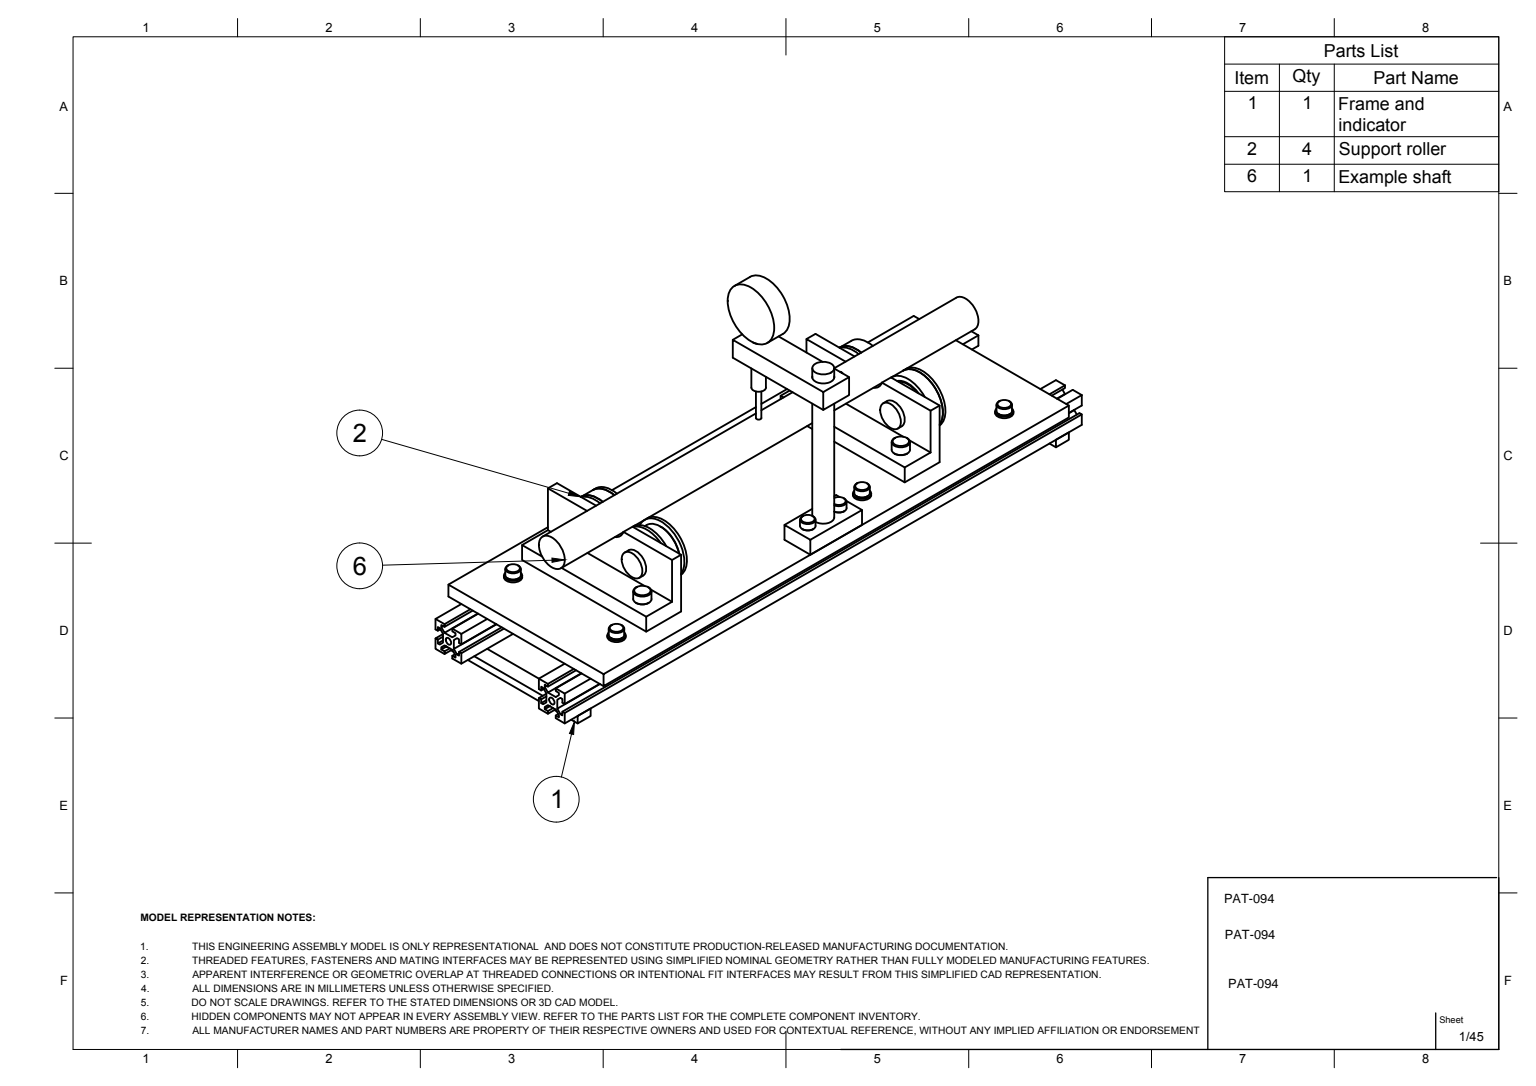
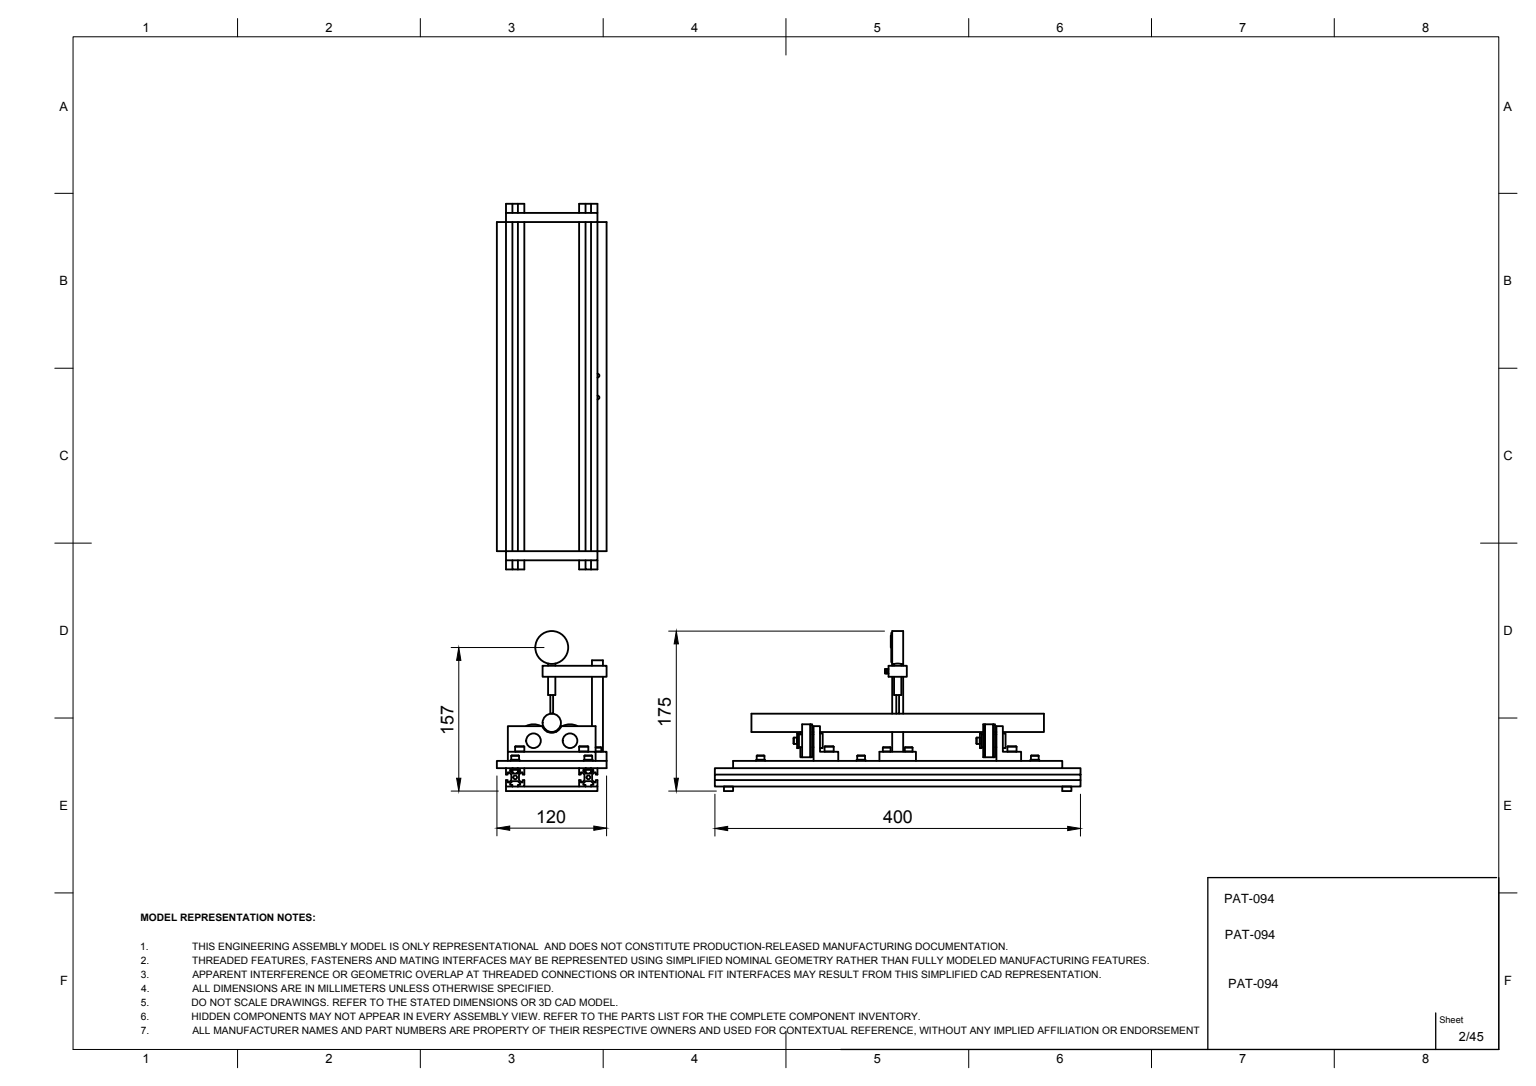
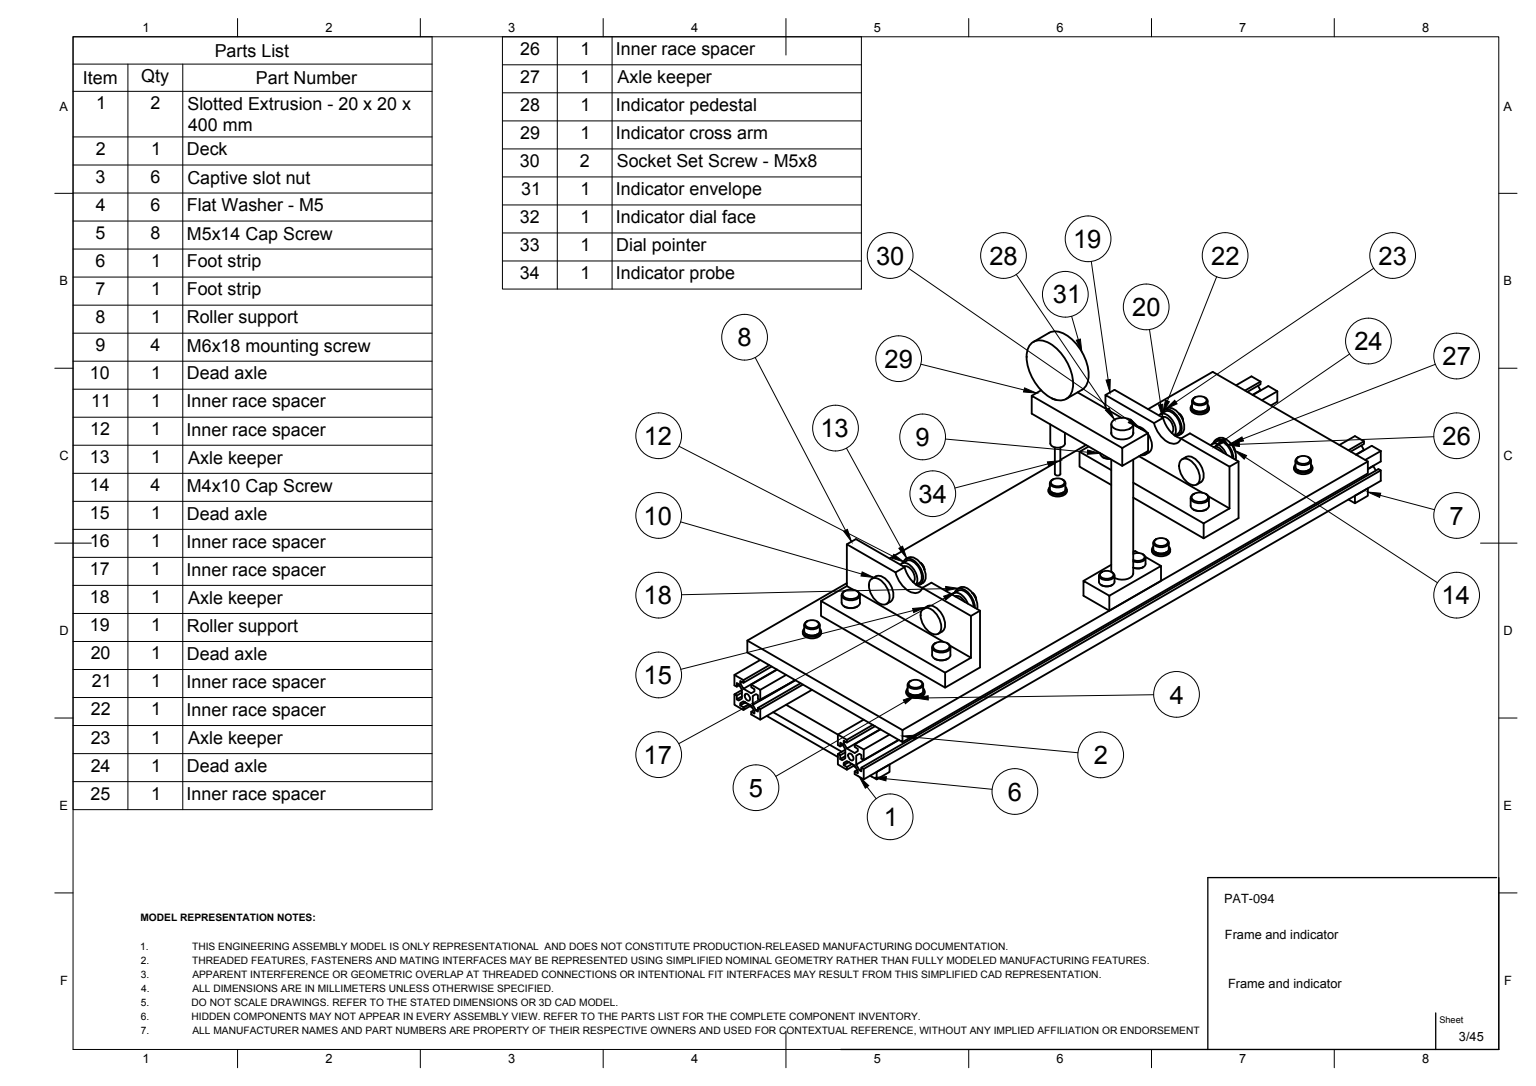
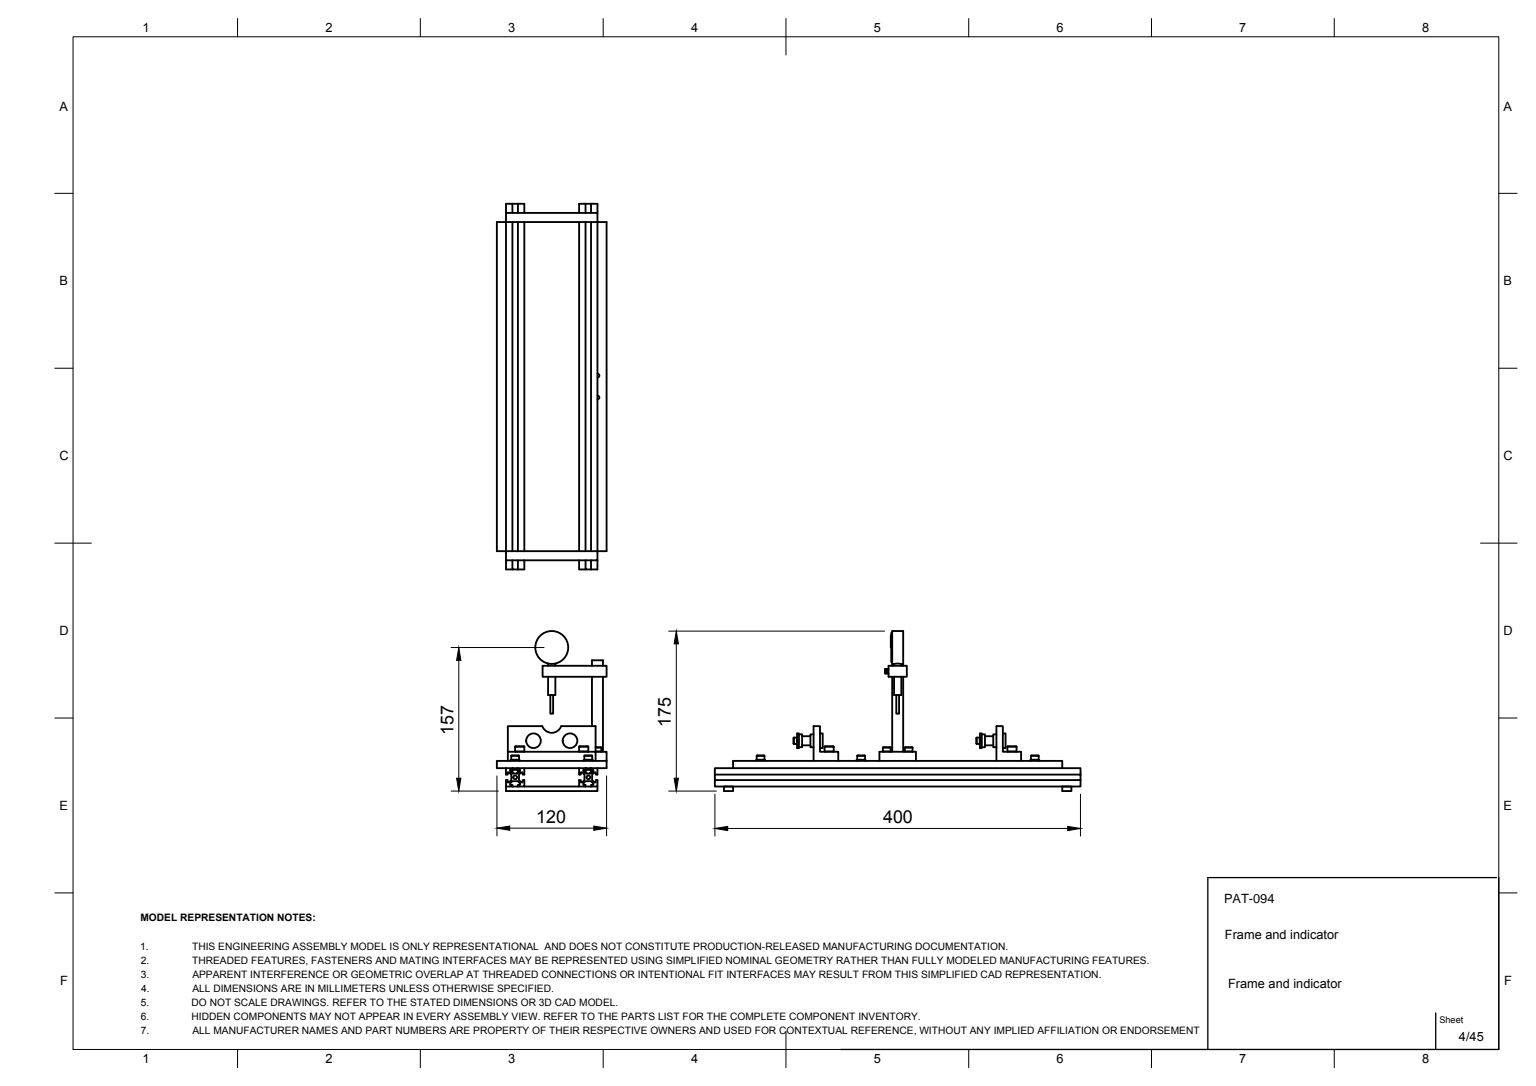
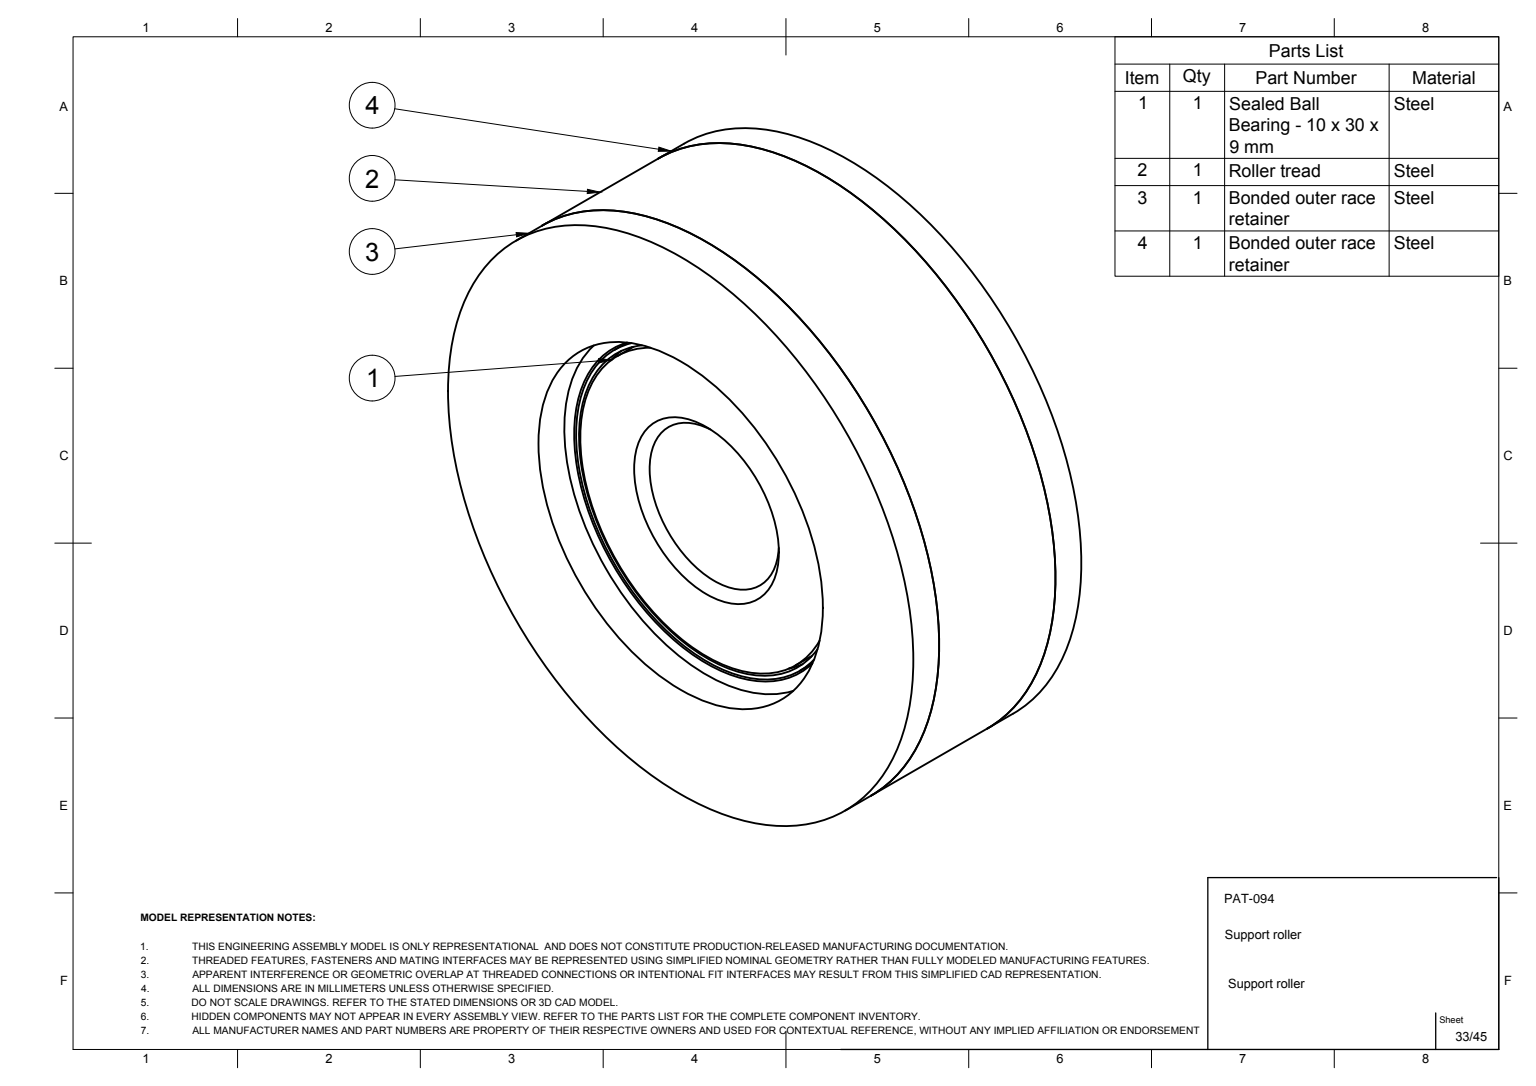
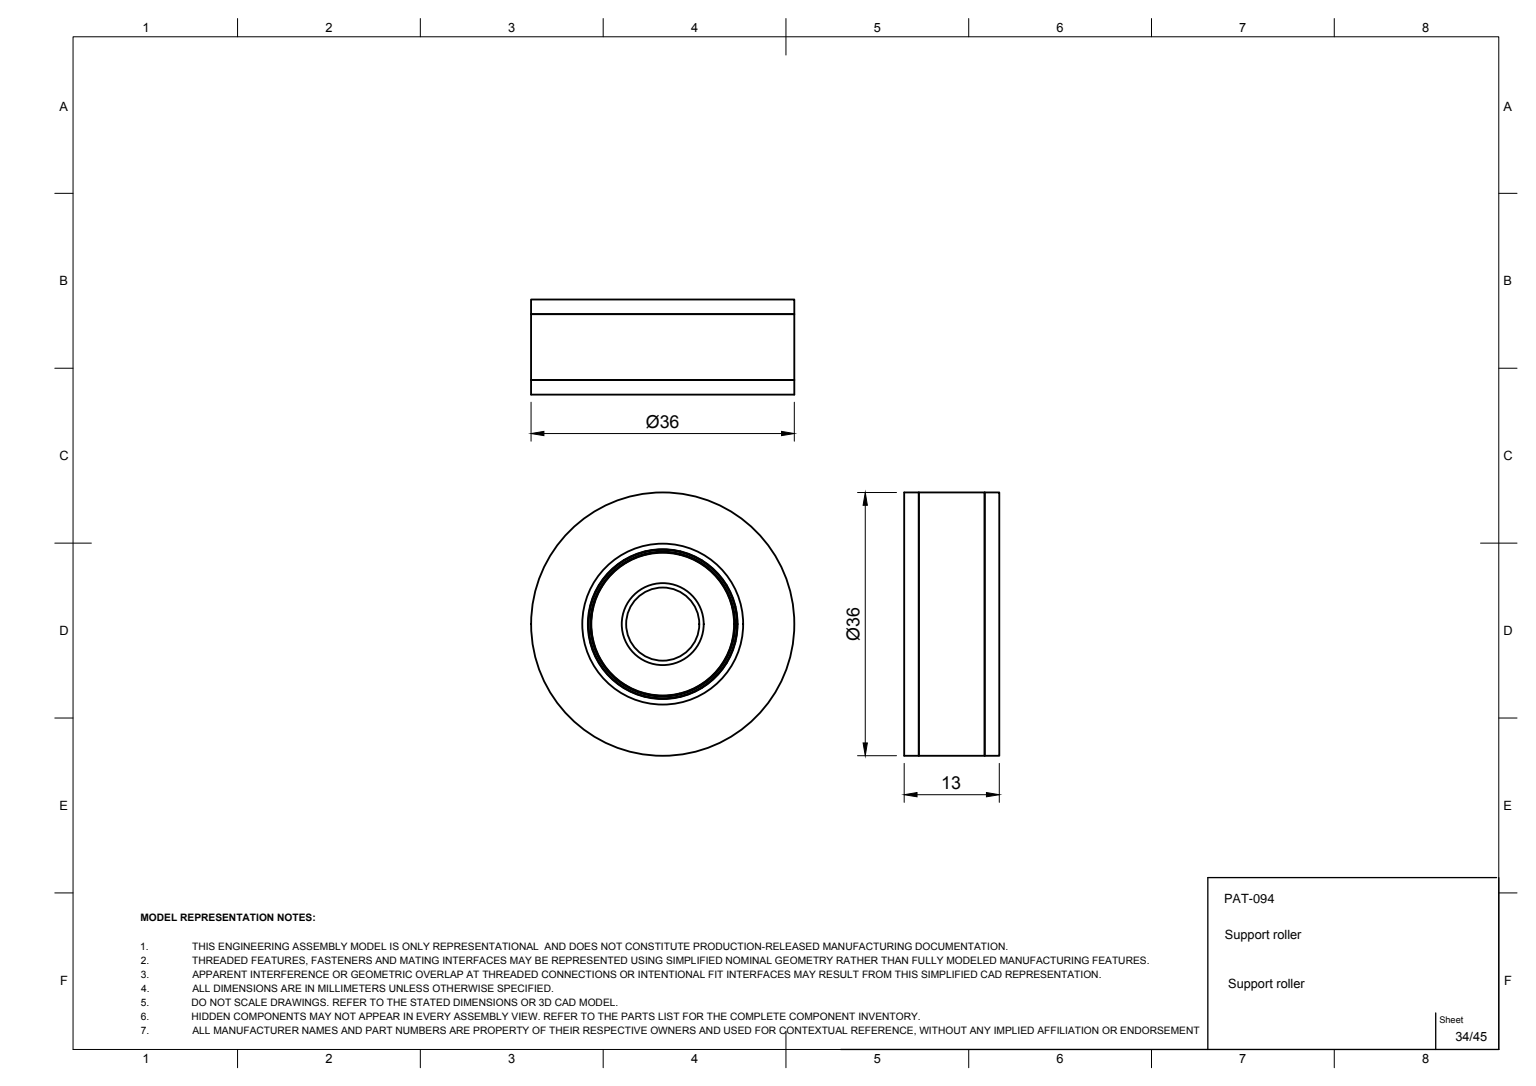
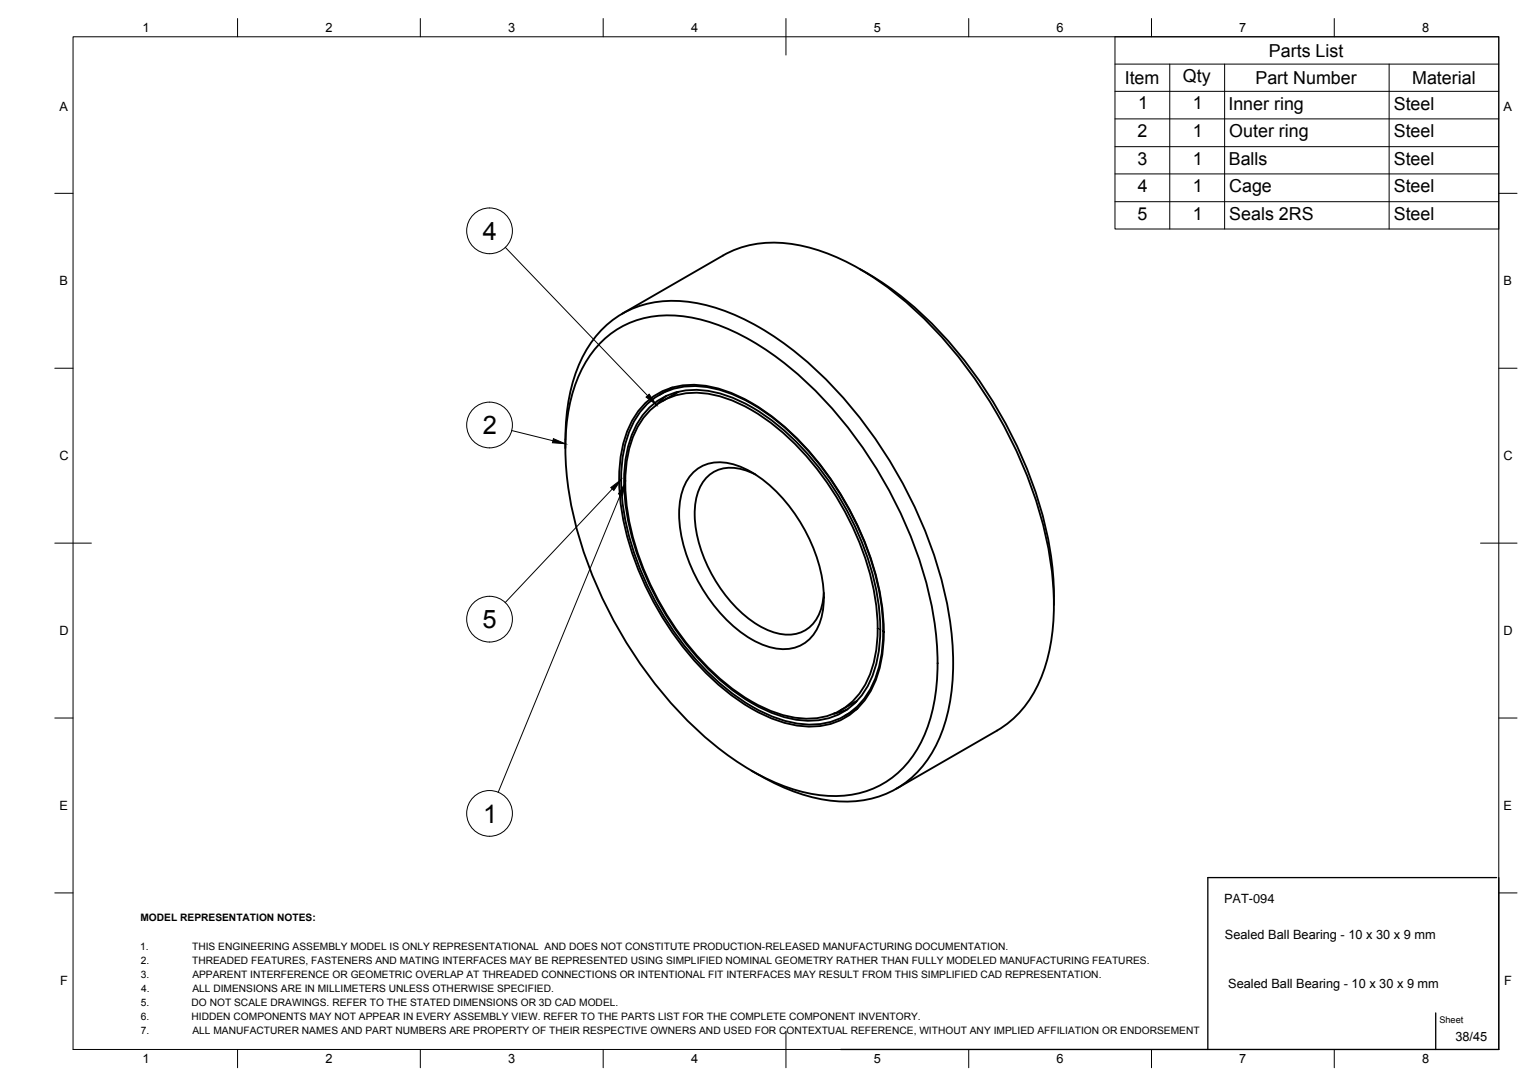
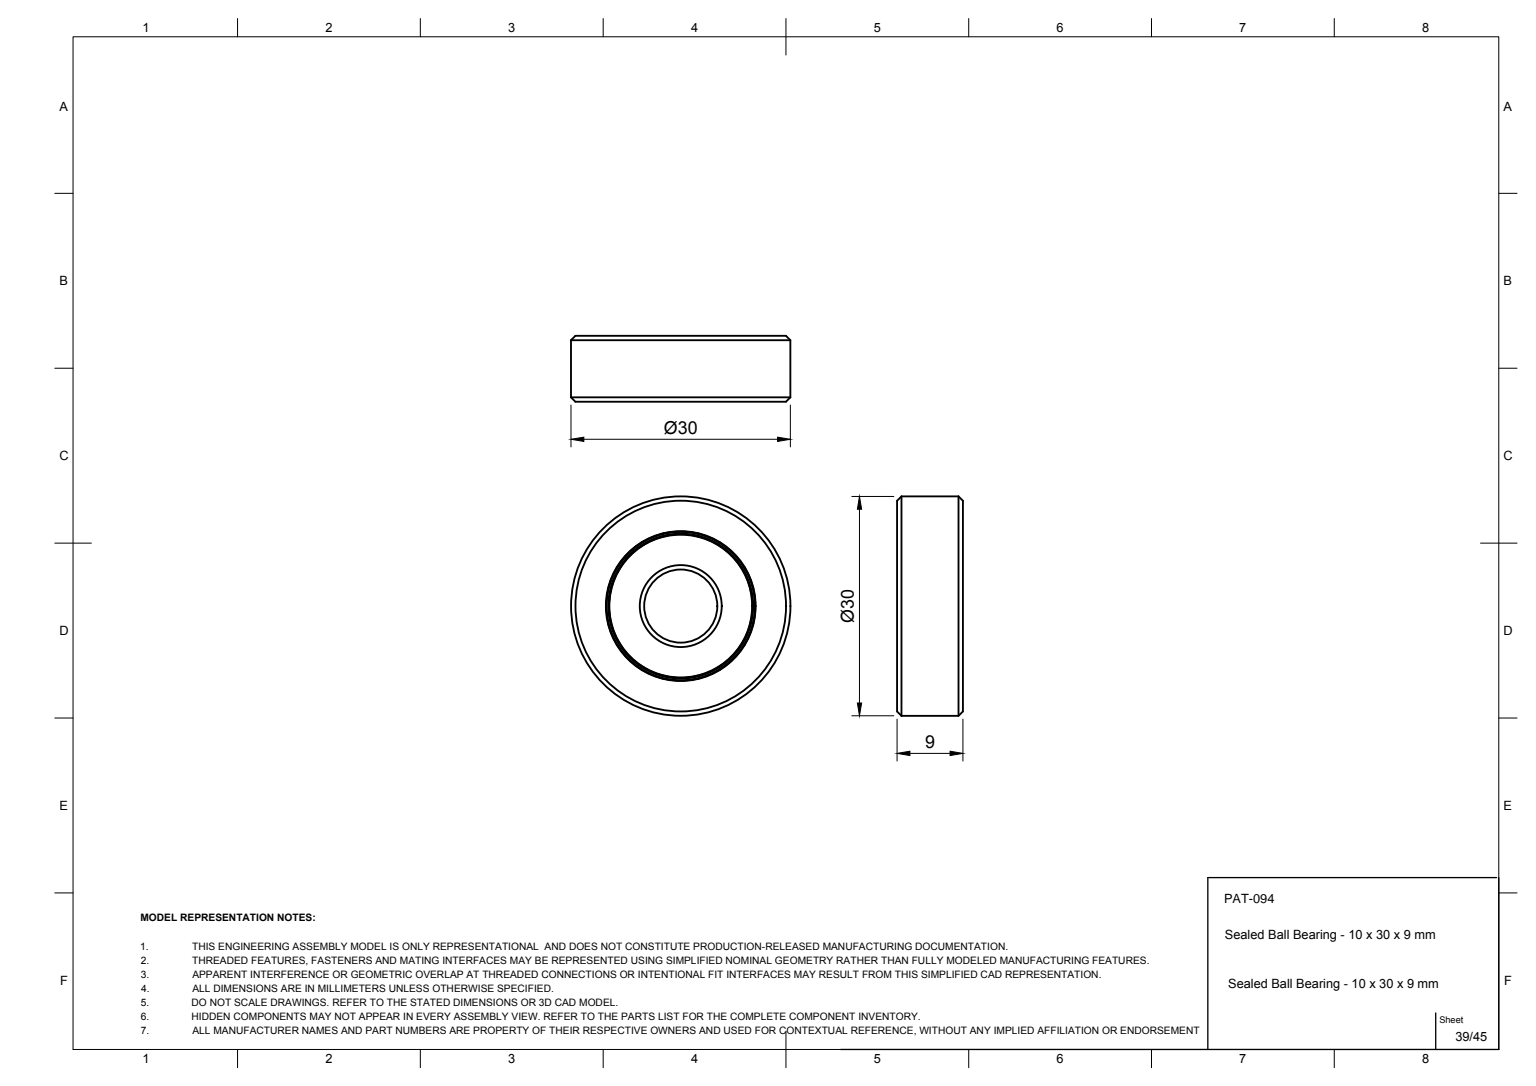
ISO-10303-21;
HEADER;
/* Generated by software containing ST-Developer
 * from STEP Tools, Inc. (www.steptools.com) 
 */

FILE_DESCRIPTION(
/* description */ ('Shaft runout checking stand'),
/* implementation_level */ '2;1');

FILE_NAME(
/* name */ 'PAT-094',
/* time_stamp */ '2026-11-02T21:12:33-08:00',
/* author */ (''),
/* organization */ (''),
/* preprocessor_version */ 'ST-DEVELOPER v20.2',
/* originating_system */ 'Autodesk Translation Framework v15.17.0.0',
/* authorisation */ '');

FILE_SCHEMA (('AUTOMOTIVE_DESIGN { 1 0 10303 214 3 1 1 }'));
ENDSEC;

DATA;
#10=MECHANICAL_DESIGN_GEOMETRIC_PRESENTATION_REPRESENTATION('',(#463,#464,
#465,#466,#467,#468,#469,#470,#471,#472,#473,#474,#475,#476,#477,#478,#479,
#480,#481,#482,#483,#484,#485,#486,#487,#488,#489,#490,#491,#492,#493,#494,
#495,#496,#497,#498,#499,#500,#501,#502,#503,#504,#505,#506,#507,#508,#509,
#510,#511,#512,#513),#11748);
#11=SPHERICAL_SURFACE('',#7363,0.23815);
#12=SPHERICAL_SURFACE('',#7365,0.23815);
#13=SPHERICAL_SURFACE('',#7367,0.23815);
#14=SPHERICAL_SURFACE('',#7369,0.23815);
#15=SPHERICAL_SURFACE('',#7371,0.23815);
#16=SPHERICAL_SURFACE('',#7373,0.23815);
#17=SPHERICAL_SURFACE('',#7375,0.23815);
#18=SPHERICAL_SURFACE('',#7377,0.23815);
#19=SPHERICAL_SURFACE('',#7380,0.247676);
#20=SPHERICAL_SURFACE('',#7396,0.247676);
#21=SPHERICAL_SURFACE('',#7401,0.247676);
#22=SPHERICAL_SURFACE('',#7406,0.247676);
#23=SPHERICAL_SURFACE('',#7411,0.247676);
#24=SPHERICAL_SURFACE('',#7416,0.247676);
#25=SPHERICAL_SURFACE('',#7421,0.247676);
#26=SPHERICAL_SURFACE('',#7429,0.247676);
#27=TOROIDAL_SURFACE('',#7323,1.,0.247676);
#28=TOROIDAL_SURFACE('',#7343,1.,0.247676);
#29=ITEM_DEFINED_TRANSFORMATION($,$,#6736,#7253);
#30=ITEM_DEFINED_TRANSFORMATION($,$,#6736,#7254);
#31=ITEM_DEFINED_TRANSFORMATION($,$,#6786,#7255);
#32=ITEM_DEFINED_TRANSFORMATION($,$,#6829,#7256);
#33=ITEM_DEFINED_TRANSFORMATION($,$,#6850,#7257);
#34=ITEM_DEFINED_TRANSFORMATION($,$,#7127,#7258);
#35=ITEM_DEFINED_TRANSFORMATION($,$,#6829,#7259);
#36=ITEM_DEFINED_TRANSFORMATION($,$,#6850,#7260);
#37=ITEM_DEFINED_TRANSFORMATION($,$,#7127,#7261);
#38=ITEM_DEFINED_TRANSFORMATION($,$,#6829,#7262);
#39=ITEM_DEFINED_TRANSFORMATION($,$,#6850,#7263);
#40=ITEM_DEFINED_TRANSFORMATION($,$,#7127,#7264);
#41=ITEM_DEFINED_TRANSFORMATION($,$,#6829,#7265);
#42=ITEM_DEFINED_TRANSFORMATION($,$,#6850,#7266);
#43=ITEM_DEFINED_TRANSFORMATION($,$,#7127,#7267);
#44=ITEM_DEFINED_TRANSFORMATION($,$,#6829,#7268);
#45=ITEM_DEFINED_TRANSFORMATION($,$,#6850,#7269);
#46=ITEM_DEFINED_TRANSFORMATION($,$,#7127,#7270);
#47=ITEM_DEFINED_TRANSFORMATION($,$,#6829,#7271);
#48=ITEM_DEFINED_TRANSFORMATION($,$,#6850,#7272);
#49=ITEM_DEFINED_TRANSFORMATION($,$,#7127,#7273);
#50=ITEM_DEFINED_TRANSFORMATION($,$,#6861,#7274);
#51=ITEM_DEFINED_TRANSFORMATION($,$,#6868,#7275);
#52=ITEM_DEFINED_TRANSFORMATION($,$,#6875,#7276);
#53=ITEM_DEFINED_TRANSFORMATION($,$,#6998,#7277);
#54=ITEM_DEFINED_TRANSFORMATION($,$,#6998,#7278);
#55=ITEM_DEFINED_TRANSFORMATION($,$,#6900,#7279);
#56=ITEM_DEFINED_TRANSFORMATION($,$,#6914,#7280);
#57=ITEM_DEFINED_TRANSFORMATION($,$,#6923,#7281);
#58=ITEM_DEFINED_TRANSFORMATION($,$,#6932,#7282);
#59=ITEM_DEFINED_TRANSFORMATION($,$,#7086,#7283);
#60=ITEM_DEFINED_TRANSFORMATION($,$,#6941,#7284);
#61=ITEM_DEFINED_TRANSFORMATION($,$,#6955,#7285);
#62=ITEM_DEFINED_TRANSFORMATION($,$,#6964,#7286);
#63=ITEM_DEFINED_TRANSFORMATION($,$,#7086,#7287);
#64=ITEM_DEFINED_TRANSFORMATION($,$,#6973,#7288);
#65=ITEM_DEFINED_TRANSFORMATION($,$,#6998,#7289);
#66=ITEM_DEFINED_TRANSFORMATION($,$,#6998,#7290);
#67=ITEM_DEFINED_TRANSFORMATION($,$,#7022,#7291);
#68=ITEM_DEFINED_TRANSFORMATION($,$,#7036,#7292);
#69=ITEM_DEFINED_TRANSFORMATION($,$,#7045,#7293);
#70=ITEM_DEFINED_TRANSFORMATION($,$,#7086,#7294);
#71=ITEM_DEFINED_TRANSFORMATION($,$,#7054,#7295);
#72=ITEM_DEFINED_TRANSFORMATION($,$,#7068,#7296);
#73=ITEM_DEFINED_TRANSFORMATION($,$,#7077,#7297);
#74=ITEM_DEFINED_TRANSFORMATION($,$,#7086,#7298);
#75=ITEM_DEFINED_TRANSFORMATION($,$,#7110,#7299);
#76=ITEM_DEFINED_TRANSFORMATION($,$,#7127,#7300);
#77=ITEM_DEFINED_TRANSFORMATION($,$,#7127,#7301);
#78=ITEM_DEFINED_TRANSFORMATION($,$,#7151,#7302);
#79=ITEM_DEFINED_TRANSFORMATION($,$,#7178,#7303);
#80=ITEM_DEFINED_TRANSFORMATION($,$,#7178,#7304);
#81=ITEM_DEFINED_TRANSFORMATION($,$,#7195,#7305);
#82=ITEM_DEFINED_TRANSFORMATION($,$,#7208,#7306);
#83=ITEM_DEFINED_TRANSFORMATION($,$,#7214,#7307);
#84=ITEM_DEFINED_TRANSFORMATION($,$,#7220,#7308);
#85=ITEM_DEFINED_TRANSFORMATION($,$,#7226,#7309);
#86=ITEM_DEFINED_TRANSFORMATION($,$,#7235,#7310);
#87=ITEM_DEFINED_TRANSFORMATION($,$,#7244,#7311);
#88=ITEM_DEFINED_TRANSFORMATION($,$,#7313,#7319);
#89=ITEM_DEFINED_TRANSFORMATION($,$,#7322,#7450);
#90=ITEM_DEFINED_TRANSFORMATION($,$,#7342,#7451);
#91=ITEM_DEFINED_TRANSFORMATION($,$,#7362,#7452);
#92=ITEM_DEFINED_TRANSFORMATION($,$,#7379,#7453);
#93=ITEM_DEFINED_TRANSFORMATION($,$,#7433,#7454);
#94=ITEM_DEFINED_TRANSFORMATION($,$,#7321,#7482);
#95=ITEM_DEFINED_TRANSFORMATION($,$,#7455,#7483);
#96=ITEM_DEFINED_TRANSFORMATION($,$,#7464,#7484);
#97=ITEM_DEFINED_TRANSFORMATION($,$,#7473,#7485);
#98=ITEM_DEFINED_TRANSFORMATION($,$,#6735,#7486);
#99=ITEM_DEFINED_TRANSFORMATION($,$,#7320,#7487);
#100=ITEM_DEFINED_TRANSFORMATION($,$,#7312,#7488);
#101=ITEM_DEFINED_TRANSFORMATION($,$,#7320,#7489);
#102=ITEM_DEFINED_TRANSFORMATION($,$,#7320,#7490);
#103=ITEM_DEFINED_TRANSFORMATION($,$,#7320,#7491);
#104=(
REPRESENTATION_RELATIONSHIP($,$,#11926,#11925)
REPRESENTATION_RELATIONSHIP_WITH_TRANSFORMATION(#29)
SHAPE_REPRESENTATION_RELATIONSHIP()
);
#105=(
REPRESENTATION_RELATIONSHIP($,$,#11926,#11925)
REPRESENTATION_RELATIONSHIP_WITH_TRANSFORMATION(#30)
SHAPE_REPRESENTATION_RELATIONSHIP()
);
#106=(
REPRESENTATION_RELATIONSHIP($,$,#11927,#11925)
REPRESENTATION_RELATIONSHIP_WITH_TRANSFORMATION(#31)
SHAPE_REPRESENTATION_RELATIONSHIP()
);
#107=(
REPRESENTATION_RELATIONSHIP($,$,#11928,#11925)
REPRESENTATION_RELATIONSHIP_WITH_TRANSFORMATION(#32)
SHAPE_REPRESENTATION_RELATIONSHIP()
);
#108=(
REPRESENTATION_RELATIONSHIP($,$,#11929,#11925)
REPRESENTATION_RELATIONSHIP_WITH_TRANSFORMATION(#33)
SHAPE_REPRESENTATION_RELATIONSHIP()
);
#109=(
REPRESENTATION_RELATIONSHIP($,$,#11950,#11925)
REPRESENTATION_RELATIONSHIP_WITH_TRANSFORMATION(#34)
SHAPE_REPRESENTATION_RELATIONSHIP()
);
#110=(
REPRESENTATION_RELATIONSHIP($,$,#11928,#11925)
REPRESENTATION_RELATIONSHIP_WITH_TRANSFORMATION(#35)
SHAPE_REPRESENTATION_RELATIONSHIP()
);
#111=(
REPRESENTATION_RELATIONSHIP($,$,#11929,#11925)
REPRESENTATION_RELATIONSHIP_WITH_TRANSFORMATION(#36)
SHAPE_REPRESENTATION_RELATIONSHIP()
);
#112=(
REPRESENTATION_RELATIONSHIP($,$,#11950,#11925)
REPRESENTATION_RELATIONSHIP_WITH_TRANSFORMATION(#37)
SHAPE_REPRESENTATION_RELATIONSHIP()
);
#113=(
REPRESENTATION_RELATIONSHIP($,$,#11928,#11925)
REPRESENTATION_RELATIONSHIP_WITH_TRANSFORMATION(#38)
SHAPE_REPRESENTATION_RELATIONSHIP()
);
#114=(
REPRESENTATION_RELATIONSHIP($,$,#11929,#11925)
REPRESENTATION_RELATIONSHIP_WITH_TRANSFORMATION(#39)
SHAPE_REPRESENTATION_RELATIONSHIP()
);
#115=(
REPRESENTATION_RELATIONSHIP($,$,#11950,#11925)
REPRESENTATION_RELATIONSHIP_WITH_TRANSFORMATION(#40)
SHAPE_REPRESENTATION_RELATIONSHIP()
);
#116=(
REPRESENTATION_RELATIONSHIP($,$,#11928,#11925)
REPRESENTATION_RELATIONSHIP_WITH_TRANSFORMATION(#41)
SHAPE_REPRESENTATION_RELATIONSHIP()
);
#117=(
REPRESENTATION_RELATIONSHIP($,$,#11929,#11925)
REPRESENTATION_RELATIONSHIP_WITH_TRANSFORMATION(#42)
SHAPE_REPRESENTATION_RELATIONSHIP()
);
#118=(
REPRESENTATION_RELATIONSHIP($,$,#11950,#11925)
REPRESENTATION_RELATIONSHIP_WITH_TRANSFORMATION(#43)
SHAPE_REPRESENTATION_RELATIONSHIP()
);
#119=(
REPRESENTATION_RELATIONSHIP($,$,#11928,#11925)
REPRESENTATION_RELATIONSHIP_WITH_TRANSFORMATION(#44)
SHAPE_REPRESENTATION_RELATIONSHIP()
);
#120=(
REPRESENTATION_RELATIONSHIP($,$,#11929,#11925)
REPRESENTATION_RELATIONSHIP_WITH_TRANSFORMATION(#45)
SHAPE_REPRESENTATION_RELATIONSHIP()
);
#121=(
REPRESENTATION_RELATIONSHIP($,$,#11950,#11925)
REPRESENTATION_RELATIONSHIP_WITH_TRANSFORMATION(#46)
SHAPE_REPRESENTATION_RELATIONSHIP()
);
#122=(
REPRESENTATION_RELATIONSHIP($,$,#11928,#11925)
REPRESENTATION_RELATIONSHIP_WITH_TRANSFORMATION(#47)
SHAPE_REPRESENTATION_RELATIONSHIP()
);
#123=(
REPRESENTATION_RELATIONSHIP($,$,#11929,#11925)
REPRESENTATION_RELATIONSHIP_WITH_TRANSFORMATION(#48)
SHAPE_REPRESENTATION_RELATIONSHIP()
);
#124=(
REPRESENTATION_RELATIONSHIP($,$,#11950,#11925)
REPRESENTATION_RELATIONSHIP_WITH_TRANSFORMATION(#49)
SHAPE_REPRESENTATION_RELATIONSHIP()
);
#125=(
REPRESENTATION_RELATIONSHIP($,$,#11930,#11925)
REPRESENTATION_RELATIONSHIP_WITH_TRANSFORMATION(#50)
SHAPE_REPRESENTATION_RELATIONSHIP()
);
#126=(
REPRESENTATION_RELATIONSHIP($,$,#11931,#11925)
REPRESENTATION_RELATIONSHIP_WITH_TRANSFORMATION(#51)
SHAPE_REPRESENTATION_RELATIONSHIP()
);
#127=(
REPRESENTATION_RELATIONSHIP($,$,#11932,#11925)
REPRESENTATION_RELATIONSHIP_WITH_TRANSFORMATION(#52)
SHAPE_REPRESENTATION_RELATIONSHIP()
);
#128=(
REPRESENTATION_RELATIONSHIP($,$,#11941,#11925)
REPRESENTATION_RELATIONSHIP_WITH_TRANSFORMATION(#53)
SHAPE_REPRESENTATION_RELATIONSHIP()
);
#129=(
REPRESENTATION_RELATIONSHIP($,$,#11941,#11925)
REPRESENTATION_RELATIONSHIP_WITH_TRANSFORMATION(#54)
SHAPE_REPRESENTATION_RELATIONSHIP()
);
#130=(
REPRESENTATION_RELATIONSHIP($,$,#11933,#11925)
REPRESENTATION_RELATIONSHIP_WITH_TRANSFORMATION(#55)
SHAPE_REPRESENTATION_RELATIONSHIP()
);
#131=(
REPRESENTATION_RELATIONSHIP($,$,#11934,#11925)
REPRESENTATION_RELATIONSHIP_WITH_TRANSFORMATION(#56)
SHAPE_REPRESENTATION_RELATIONSHIP()
);
#132=(
REPRESENTATION_RELATIONSHIP($,$,#11935,#11925)
REPRESENTATION_RELATIONSHIP_WITH_TRANSFORMATION(#57)
SHAPE_REPRESENTATION_RELATIONSHIP()
);
#133=(
REPRESENTATION_RELATIONSHIP($,$,#11936,#11925)
REPRESENTATION_RELATIONSHIP_WITH_TRANSFORMATION(#58)
SHAPE_REPRESENTATION_RELATIONSHIP()
);
#134=(
REPRESENTATION_RELATIONSHIP($,$,#11948,#11925)
REPRESENTATION_RELATIONSHIP_WITH_TRANSFORMATION(#59)
SHAPE_REPRESENTATION_RELATIONSHIP()
);
#135=(
REPRESENTATION_RELATIONSHIP($,$,#11937,#11925)
REPRESENTATION_RELATIONSHIP_WITH_TRANSFORMATION(#60)
SHAPE_REPRESENTATION_RELATIONSHIP()
);
#136=(
REPRESENTATION_RELATIONSHIP($,$,#11938,#11925)
REPRESENTATION_RELATIONSHIP_WITH_TRANSFORMATION(#61)
SHAPE_REPRESENTATION_RELATIONSHIP()
);
#137=(
REPRESENTATION_RELATIONSHIP($,$,#11939,#11925)
REPRESENTATION_RELATIONSHIP_WITH_TRANSFORMATION(#62)
SHAPE_REPRESENTATION_RELATIONSHIP()
);
#138=(
REPRESENTATION_RELATIONSHIP($,$,#11948,#11925)
REPRESENTATION_RELATIONSHIP_WITH_TRANSFORMATION(#63)
SHAPE_REPRESENTATION_RELATIONSHIP()
);
#139=(
REPRESENTATION_RELATIONSHIP($,$,#11940,#11925)
REPRESENTATION_RELATIONSHIP_WITH_TRANSFORMATION(#64)
SHAPE_REPRESENTATION_RELATIONSHIP()
);
#140=(
REPRESENTATION_RELATIONSHIP($,$,#11941,#11925)
REPRESENTATION_RELATIONSHIP_WITH_TRANSFORMATION(#65)
SHAPE_REPRESENTATION_RELATIONSHIP()
);
#141=(
REPRESENTATION_RELATIONSHIP($,$,#11941,#11925)
REPRESENTATION_RELATIONSHIP_WITH_TRANSFORMATION(#66)
SHAPE_REPRESENTATION_RELATIONSHIP()
);
#142=(
REPRESENTATION_RELATIONSHIP($,$,#11942,#11925)
REPRESENTATION_RELATIONSHIP_WITH_TRANSFORMATION(#67)
SHAPE_REPRESENTATION_RELATIONSHIP()
);
#143=(
REPRESENTATION_RELATIONSHIP($,$,#11943,#11925)
REPRESENTATION_RELATIONSHIP_WITH_TRANSFORMATION(#68)
SHAPE_REPRESENTATION_RELATIONSHIP()
);
#144=(
REPRESENTATION_RELATIONSHIP($,$,#11944,#11925)
REPRESENTATION_RELATIONSHIP_WITH_TRANSFORMATION(#69)
SHAPE_REPRESENTATION_RELATIONSHIP()
);
#145=(
REPRESENTATION_RELATIONSHIP($,$,#11948,#11925)
REPRESENTATION_RELATIONSHIP_WITH_TRANSFORMATION(#70)
SHAPE_REPRESENTATION_RELATIONSHIP()
);
#146=(
REPRESENTATION_RELATIONSHIP($,$,#11945,#11925)
REPRESENTATION_RELATIONSHIP_WITH_TRANSFORMATION(#71)
SHAPE_REPRESENTATION_RELATIONSHIP()
);
#147=(
REPRESENTATION_RELATIONSHIP($,$,#11946,#11925)
REPRESENTATION_RELATIONSHIP_WITH_TRANSFORMATION(#72)
SHAPE_REPRESENTATION_RELATIONSHIP()
);
#148=(
REPRESENTATION_RELATIONSHIP($,$,#11947,#11925)
REPRESENTATION_RELATIONSHIP_WITH_TRANSFORMATION(#73)
SHAPE_REPRESENTATION_RELATIONSHIP()
);
#149=(
REPRESENTATION_RELATIONSHIP($,$,#11948,#11925)
REPRESENTATION_RELATIONSHIP_WITH_TRANSFORMATION(#74)
SHAPE_REPRESENTATION_RELATIONSHIP()
);
#150=(
REPRESENTATION_RELATIONSHIP($,$,#11949,#11925)
REPRESENTATION_RELATIONSHIP_WITH_TRANSFORMATION(#75)
SHAPE_REPRESENTATION_RELATIONSHIP()
);
#151=(
REPRESENTATION_RELATIONSHIP($,$,#11950,#11925)
REPRESENTATION_RELATIONSHIP_WITH_TRANSFORMATION(#76)
SHAPE_REPRESENTATION_RELATIONSHIP()
);
#152=(
REPRESENTATION_RELATIONSHIP($,$,#11950,#11925)
REPRESENTATION_RELATIONSHIP_WITH_TRANSFORMATION(#77)
SHAPE_REPRESENTATION_RELATIONSHIP()
);
#153=(
REPRESENTATION_RELATIONSHIP($,$,#11951,#11925)
REPRESENTATION_RELATIONSHIP_WITH_TRANSFORMATION(#78)
SHAPE_REPRESENTATION_RELATIONSHIP()
);
#154=(
REPRESENTATION_RELATIONSHIP($,$,#11952,#11925)
REPRESENTATION_RELATIONSHIP_WITH_TRANSFORMATION(#79)
SHAPE_REPRESENTATION_RELATIONSHIP()
);
#155=(
REPRESENTATION_RELATIONSHIP($,$,#11952,#11925)
REPRESENTATION_RELATIONSHIP_WITH_TRANSFORMATION(#80)
SHAPE_REPRESENTATION_RELATIONSHIP()
);
#156=(
REPRESENTATION_RELATIONSHIP($,$,#11953,#11925)
REPRESENTATION_RELATIONSHIP_WITH_TRANSFORMATION(#81)
SHAPE_REPRESENTATION_RELATIONSHIP()
);
#157=(
REPRESENTATION_RELATIONSHIP($,$,#11954,#11925)
REPRESENTATION_RELATIONSHIP_WITH_TRANSFORMATION(#82)
SHAPE_REPRESENTATION_RELATIONSHIP()
);
#158=(
REPRESENTATION_RELATIONSHIP($,$,#11955,#11925)
REPRESENTATION_RELATIONSHIP_WITH_TRANSFORMATION(#83)
SHAPE_REPRESENTATION_RELATIONSHIP()
);
#159=(
REPRESENTATION_RELATIONSHIP($,$,#11956,#11925)
REPRESENTATION_RELATIONSHIP_WITH_TRANSFORMATION(#84)
SHAPE_REPRESENTATION_RELATIONSHIP()
);
#160=(
REPRESENTATION_RELATIONSHIP($,$,#11957,#11925)
REPRESENTATION_RELATIONSHIP_WITH_TRANSFORMATION(#85)
SHAPE_REPRESENTATION_RELATIONSHIP()
);
#161=(
REPRESENTATION_RELATIONSHIP($,$,#11958,#11925)
REPRESENTATION_RELATIONSHIP_WITH_TRANSFORMATION(#86)
SHAPE_REPRESENTATION_RELATIONSHIP()
);
#162=(
REPRESENTATION_RELATIONSHIP($,$,#11959,#11925)
REPRESENTATION_RELATIONSHIP_WITH_TRANSFORMATION(#87)
SHAPE_REPRESENTATION_RELATIONSHIP()
);
#163=(
REPRESENTATION_RELATIONSHIP($,$,#11961,#11960)
REPRESENTATION_RELATIONSHIP_WITH_TRANSFORMATION(#88)
SHAPE_REPRESENTATION_RELATIONSHIP()
);
#164=(
REPRESENTATION_RELATIONSHIP($,$,#11964,#11963)
REPRESENTATION_RELATIONSHIP_WITH_TRANSFORMATION(#89)
SHAPE_REPRESENTATION_RELATIONSHIP()
);
#165=(
REPRESENTATION_RELATIONSHIP($,$,#11965,#11963)
REPRESENTATION_RELATIONSHIP_WITH_TRANSFORMATION(#90)
SHAPE_REPRESENTATION_RELATIONSHIP()
);
#166=(
REPRESENTATION_RELATIONSHIP($,$,#11966,#11963)
REPRESENTATION_RELATIONSHIP_WITH_TRANSFORMATION(#91)
SHAPE_REPRESENTATION_RELATIONSHIP()
);
#167=(
REPRESENTATION_RELATIONSHIP($,$,#11967,#11963)
REPRESENTATION_RELATIONSHIP_WITH_TRANSFORMATION(#92)
SHAPE_REPRESENTATION_RELATIONSHIP()
);
#168=(
REPRESENTATION_RELATIONSHIP($,$,#11968,#11963)
REPRESENTATION_RELATIONSHIP_WITH_TRANSFORMATION(#93)
SHAPE_REPRESENTATION_RELATIONSHIP()
);
#169=(
REPRESENTATION_RELATIONSHIP($,$,#11963,#11962)
REPRESENTATION_RELATIONSHIP_WITH_TRANSFORMATION(#94)
SHAPE_REPRESENTATION_RELATIONSHIP()
);
#170=(
REPRESENTATION_RELATIONSHIP($,$,#11969,#11962)
REPRESENTATION_RELATIONSHIP_WITH_TRANSFORMATION(#95)
SHAPE_REPRESENTATION_RELATIONSHIP()
);
#171=(
REPRESENTATION_RELATIONSHIP($,$,#11970,#11962)
REPRESENTATION_RELATIONSHIP_WITH_TRANSFORMATION(#96)
SHAPE_REPRESENTATION_RELATIONSHIP()
);
#172=(
REPRESENTATION_RELATIONSHIP($,$,#11971,#11962)
REPRESENTATION_RELATIONSHIP_WITH_TRANSFORMATION(#97)
SHAPE_REPRESENTATION_RELATIONSHIP()
);
#173=(
REPRESENTATION_RELATIONSHIP($,$,#11925,#11924)
REPRESENTATION_RELATIONSHIP_WITH_TRANSFORMATION(#98)
SHAPE_REPRESENTATION_RELATIONSHIP()
);
#174=(
REPRESENTATION_RELATIONSHIP($,$,#11962,#11924)
REPRESENTATION_RELATIONSHIP_WITH_TRANSFORMATION(#99)
SHAPE_REPRESENTATION_RELATIONSHIP()
);
#175=(
REPRESENTATION_RELATIONSHIP($,$,#11960,#11924)
REPRESENTATION_RELATIONSHIP_WITH_TRANSFORMATION(#100)
SHAPE_REPRESENTATION_RELATIONSHIP()
);
#176=(
REPRESENTATION_RELATIONSHIP($,$,#11962,#11924)
REPRESENTATION_RELATIONSHIP_WITH_TRANSFORMATION(#101)
SHAPE_REPRESENTATION_RELATIONSHIP()
);
#177=(
REPRESENTATION_RELATIONSHIP($,$,#11962,#11924)
REPRESENTATION_RELATIONSHIP_WITH_TRANSFORMATION(#102)
SHAPE_REPRESENTATION_RELATIONSHIP()
);
#178=(
REPRESENTATION_RELATIONSHIP($,$,#11962,#11924)
REPRESENTATION_RELATIONSHIP_WITH_TRANSFORMATION(#103)
SHAPE_REPRESENTATION_RELATIONSHIP()
);
#179=CONTEXT_DEPENDENT_SHAPE_REPRESENTATION(#104,#11837);
#180=CONTEXT_DEPENDENT_SHAPE_REPRESENTATION(#105,#11838);
#181=CONTEXT_DEPENDENT_SHAPE_REPRESENTATION(#106,#11839);
#182=CONTEXT_DEPENDENT_SHAPE_REPRESENTATION(#107,#11840);
#183=CONTEXT_DEPENDENT_SHAPE_REPRESENTATION(#108,#11841);
#184=CONTEXT_DEPENDENT_SHAPE_REPRESENTATION(#109,#11842);
#185=CONTEXT_DEPENDENT_SHAPE_REPRESENTATION(#110,#11843);
#186=CONTEXT_DEPENDENT_SHAPE_REPRESENTATION(#111,#11844);
#187=CONTEXT_DEPENDENT_SHAPE_REPRESENTATION(#112,#11845);
#188=CONTEXT_DEPENDENT_SHAPE_REPRESENTATION(#113,#11846);
#189=CONTEXT_DEPENDENT_SHAPE_REPRESENTATION(#114,#11847);
#190=CONTEXT_DEPENDENT_SHAPE_REPRESENTATION(#115,#11848);
#191=CONTEXT_DEPENDENT_SHAPE_REPRESENTATION(#116,#11849);
#192=CONTEXT_DEPENDENT_SHAPE_REPRESENTATION(#117,#11850);
#193=CONTEXT_DEPENDENT_SHAPE_REPRESENTATION(#118,#11851);
#194=CONTEXT_DEPENDENT_SHAPE_REPRESENTATION(#119,#11852);
#195=CONTEXT_DEPENDENT_SHAPE_REPRESENTATION(#120,#11853);
#196=CONTEXT_DEPENDENT_SHAPE_REPRESENTATION(#121,#11854);
#197=CONTEXT_DEPENDENT_SHAPE_REPRESENTATION(#122,#11855);
#198=CONTEXT_DEPENDENT_SHAPE_REPRESENTATION(#123,#11856);
#199=CONTEXT_DEPENDENT_SHAPE_REPRESENTATION(#124,#11857);
#200=CONTEXT_DEPENDENT_SHAPE_REPRESENTATION(#125,#11858);
#201=CONTEXT_DEPENDENT_SHAPE_REPRESENTATION(#126,#11859);
#202=CONTEXT_DEPENDENT_SHAPE_REPRESENTATION(#127,#11860);
#203=CONTEXT_DEPENDENT_SHAPE_REPRESENTATION(#128,#11861);
#204=CONTEXT_DEPENDENT_SHAPE_REPRESENTATION(#129,#11862);
#205=CONTEXT_DEPENDENT_SHAPE_REPRESENTATION(#130,#11863);
#206=CONTEXT_DEPENDENT_SHAPE_REPRESENTATION(#131,#11864);
#207=CONTEXT_DEPENDENT_SHAPE_REPRESENTATION(#132,#11865);
#208=CONTEXT_DEPENDENT_SHAPE_REPRESENTATION(#133,#11866);
#209=CONTEXT_DEPENDENT_SHAPE_REPRESENTATION(#134,#11867);
#210=CONTEXT_DEPENDENT_SHAPE_REPRESENTATION(#135,#11868);
#211=CONTEXT_DEPENDENT_SHAPE_REPRESENTATION(#136,#11869);
#212=CONTEXT_DEPENDENT_SHAPE_REPRESENTATION(#137,#11870);
#213=CONTEXT_DEPENDENT_SHAPE_REPRESENTATION(#138,#11871);
#214=CONTEXT_DEPENDENT_SHAPE_REPRESENTATION(#139,#11872);
#215=CONTEXT_DEPENDENT_SHAPE_REPRESENTATION(#140,#11873);
#216=CONTEXT_DEPENDENT_SHAPE_REPRESENTATION(#141,#11874);
#217=CONTEXT_DEPENDENT_SHAPE_REPRESENTATION(#142,#11875);
#218=CONTEXT_DEPENDENT_SHAPE_REPRESENTATION(#143,#11876);
#219=CONTEXT_DEPENDENT_SHAPE_REPRESENTATION(#144,#11877);
#220=CONTEXT_DEPENDENT_SHAPE_REPRESENTATION(#145,#11878);
#221=CONTEXT_DEPENDENT_SHAPE_REPRESENTATION(#146,#11879);
#222=CONTEXT_DEPENDENT_SHAPE_REPRESENTATION(#147,#11880);
#223=CONTEXT_DEPENDENT_SHAPE_REPRESENTATION(#148,#11881);
#224=CONTEXT_DEPENDENT_SHAPE_REPRESENTATION(#149,#11882);
#225=CONTEXT_DEPENDENT_SHAPE_REPRESENTATION(#150,#11883);
#226=CONTEXT_DEPENDENT_SHAPE_REPRESENTATION(#151,#11884);
#227=CONTEXT_DEPENDENT_SHAPE_REPRESENTATION(#152,#11885);
#228=CONTEXT_DEPENDENT_SHAPE_REPRESENTATION(#153,#11886);
#229=CONTEXT_DEPENDENT_SHAPE_REPRESENTATION(#154,#11887);
#230=CONTEXT_DEPENDENT_SHAPE_REPRESENTATION(#155,#11888);
#231=CONTEXT_DEPENDENT_SHAPE_REPRESENTATION(#156,#11889);
#232=CONTEXT_DEPENDENT_SHAPE_REPRESENTATION(#157,#11890);
#233=CONTEXT_DEPENDENT_SHAPE_REPRESENTATION(#158,#11891);
#234=CONTEXT_DEPENDENT_SHAPE_REPRESENTATION(#159,#11892);
#235=CONTEXT_DEPENDENT_SHAPE_REPRESENTATION(#160,#11893);
#236=CONTEXT_DEPENDENT_SHAPE_REPRESENTATION(#161,#11894);
#237=CONTEXT_DEPENDENT_SHAPE_REPRESENTATION(#162,#11895);
#238=CONTEXT_DEPENDENT_SHAPE_REPRESENTATION(#163,#11898);
#239=CONTEXT_DEPENDENT_SHAPE_REPRESENTATION(#164,#11906);
#240=CONTEXT_DEPENDENT_SHAPE_REPRESENTATION(#165,#11907);
#241=CONTEXT_DEPENDENT_SHAPE_REPRESENTATION(#166,#11908);
#242=CONTEXT_DEPENDENT_SHAPE_REPRESENTATION(#167,#11909);
#243=CONTEXT_DEPENDENT_SHAPE_REPRESENTATION(#168,#11910);
#244=CONTEXT_DEPENDENT_SHAPE_REPRESENTATION(#169,#11914);
#245=CONTEXT_DEPENDENT_SHAPE_REPRESENTATION(#170,#11915);
#246=CONTEXT_DEPENDENT_SHAPE_REPRESENTATION(#171,#11916);
#247=CONTEXT_DEPENDENT_SHAPE_REPRESENTATION(#172,#11917);
#248=CONTEXT_DEPENDENT_SHAPE_REPRESENTATION(#173,#11918);
#249=CONTEXT_DEPENDENT_SHAPE_REPRESENTATION(#174,#11919);
#250=CONTEXT_DEPENDENT_SHAPE_REPRESENTATION(#175,#11920);
#251=CONTEXT_DEPENDENT_SHAPE_REPRESENTATION(#176,#11921);
#252=CONTEXT_DEPENDENT_SHAPE_REPRESENTATION(#177,#11922);
#253=CONTEXT_DEPENDENT_SHAPE_REPRESENTATION(#178,#11923);
#254=NEXT_ASSEMBLY_USAGE_OCCURRENCE(
'Slotted Extrusion - 20 x 20 x 400 mm:2',
'Slotted Extrusion - 20 x 20 x 400 mm:2',
'Slotted Extrusion - 20 x 20 x 400 mm:2',#11974,#11975,
'Slotted Extrusion - 20 x 20 x 400 mm:2');
#255=NEXT_ASSEMBLY_USAGE_OCCURRENCE(
'Slotted Extrusion - 20 x 20 x 400 mm:3',
'Slotted Extrusion - 20 x 20 x 400 mm:3',
'Slotted Extrusion - 20 x 20 x 400 mm:3',#11974,#11975,
'Slotted Extrusion - 20 x 20 x 400 mm:3');
#256=NEXT_ASSEMBLY_USAGE_OCCURRENCE('Deck:1','Deck:1','Deck:1',#11974,#11976,
'Deck:1');
#257=NEXT_ASSEMBLY_USAGE_OCCURRENCE('Captive slot nut:2',
'Captive slot nut:2','Captive slot nut:2',#11974,#11977,
'Captive slot nut:2');
#258=NEXT_ASSEMBLY_USAGE_OCCURRENCE('Flat Washer - M5:2',
'Flat Washer - M5:2','Flat Washer - M5:2',#11974,#11978,
'Flat Washer - M5:2');
#259=NEXT_ASSEMBLY_USAGE_OCCURRENCE('M5x14 Cap Screw:2',
'M5x14 Cap Screw:2','M5x14 Cap Screw:2',#11974,#11999,
'M5x14 Cap Screw:2');
#260=NEXT_ASSEMBLY_USAGE_OCCURRENCE('Captive slot nut:3',
'Captive slot nut:3','Captive slot nut:3',#11974,#11977,
'Captive slot nut:3');
#261=NEXT_ASSEMBLY_USAGE_OCCURRENCE('Flat Washer - M5:3',
'Flat Washer - M5:3','Flat Washer - M5:3',#11974,#11978,
'Flat Washer - M5:3');
#262=NEXT_ASSEMBLY_USAGE_OCCURRENCE('M5x14 Cap Screw:3',
'M5x14 Cap Screw:3','M5x14 Cap Screw:3',#11974,#11999,
'M5x14 Cap Screw:3');
#263=NEXT_ASSEMBLY_USAGE_OCCURRENCE('Captive slot nut:4',
'Captive slot nut:4','Captive slot nut:4',#11974,#11977,
'Captive slot nut:4');
#264=NEXT_ASSEMBLY_USAGE_OCCURRENCE('Flat Washer - M5:4',
'Flat Washer - M5:4','Flat Washer - M5:4',#11974,#11978,
'Flat Washer - M5:4');
#265=NEXT_ASSEMBLY_USAGE_OCCURRENCE('M5x14 Cap Screw:4',
'M5x14 Cap Screw:4','M5x14 Cap Screw:4',#11974,#11999,
'M5x14 Cap Screw:4');
#266=NEXT_ASSEMBLY_USAGE_OCCURRENCE('Captive slot nut:5',
'Captive slot nut:5','Captive slot nut:5',#11974,#11977,
'Captive slot nut:5');
#267=NEXT_ASSEMBLY_USAGE_OCCURRENCE('Flat Washer - M5:5',
'Flat Washer - M5:5','Flat Washer - M5:5',#11974,#11978,
'Flat Washer - M5:5');
#268=NEXT_ASSEMBLY_USAGE_OCCURRENCE('M5x14 Cap Screw:5',
'M5x14 Cap Screw:5','M5x14 Cap Screw:5',#11974,#11999,
'M5x14 Cap Screw:5');
#269=NEXT_ASSEMBLY_USAGE_OCCURRENCE('Captive slot nut:6',
'Captive slot nut:6','Captive slot nut:6',#11974,#11977,
'Captive slot nut:6');
#270=NEXT_ASSEMBLY_USAGE_OCCURRENCE('Flat Washer - M5:6',
'Flat Washer - M5:6','Flat Washer - M5:6',#11974,#11978,
'Flat Washer - M5:6');
#271=NEXT_ASSEMBLY_USAGE_OCCURRENCE('M5x14 Cap Screw:6',
'M5x14 Cap Screw:6','M5x14 Cap Screw:6',#11974,#11999,
'M5x14 Cap Screw:6');
#272=NEXT_ASSEMBLY_USAGE_OCCURRENCE('Captive slot nut:7',
'Captive slot nut:7','Captive slot nut:7',#11974,#11977,
'Captive slot nut:7');
#273=NEXT_ASSEMBLY_USAGE_OCCURRENCE('Flat Washer - M5:7',
'Flat Washer - M5:7','Flat Washer - M5:7',#11974,#11978,
'Flat Washer - M5:7');
#274=NEXT_ASSEMBLY_USAGE_OCCURRENCE('M5x14 Cap Screw:7',
'M5x14 Cap Screw:7','M5x14 Cap Screw:7',#11974,#11999,
'M5x14 Cap Screw:7');
#275=NEXT_ASSEMBLY_USAGE_OCCURRENCE('Foot strip:1','Foot strip:1',
'Foot strip:1',#11974,#11979,'Foot strip:1');
#276=NEXT_ASSEMBLY_USAGE_OCCURRENCE('Foot strip (1):1',
'Foot strip (1):1','Foot strip (1):1',#11974,#11980,'Foot strip (1):1');
#277=NEXT_ASSEMBLY_USAGE_OCCURRENCE('Roller support:1',
'Roller support:1','Roller support:1',#11974,#11981,'Roller support:1');
#278=NEXT_ASSEMBLY_USAGE_OCCURRENCE('M6x18 mounting screw:2',
'M6x18 mounting screw:2','M6x18 mounting screw:2',#11974,#11990,
'M6x18 mounting screw:2');
#279=NEXT_ASSEMBLY_USAGE_OCCURRENCE('M6x18 mounting screw:3',
'M6x18 mounting screw:3','M6x18 mounting screw:3',#11974,#11990,
'M6x18 mounting screw:3');
#280=NEXT_ASSEMBLY_USAGE_OCCURRENCE('Dead axle:1','Dead axle:1',
'Dead axle:1',#11974,#11982,'Dead axle:1');
#281=NEXT_ASSEMBLY_USAGE_OCCURRENCE('Inner race spacer:1',
'Inner race spacer:1','Inner race spacer:1',#11974,#11983,
'Inner race spacer:1');
#282=NEXT_ASSEMBLY_USAGE_OCCURRENCE('Inner race spacer (1):1',
'Inner race spacer (1):1','Inner race spacer (1):1',#11974,#11984,
'Inner race spacer (1):1');
#283=NEXT_ASSEMBLY_USAGE_OCCURRENCE('Axle keeper:1','Axle keeper:1',
'Axle keeper:1',#11974,#11985,'Axle keeper:1');
#284=NEXT_ASSEMBLY_USAGE_OCCURRENCE('M4x10 Cap Screw:2',
'M4x10 Cap Screw:2','M4x10 Cap Screw:2',#11974,#11997,
'M4x10 Cap Screw:2');
#285=NEXT_ASSEMBLY_USAGE_OCCURRENCE('Dead axle (1):1','Dead axle (1):1',
'Dead axle (1):1',#11974,#11986,'Dead axle (1):1');
#286=NEXT_ASSEMBLY_USAGE_OCCURRENCE('Inner race spacer (3):1',
'Inner race spacer (3):1','Inner race spacer (3):1',#11974,#11987,
'Inner race spacer (3):1');
#287=NEXT_ASSEMBLY_USAGE_OCCURRENCE('Axle keeper (1):1',
'Axle keeper (1):1','Axle keeper (1):1',#11974,#11988,
'Axle keeper (1):1');
#288=NEXT_ASSEMBLY_USAGE_OCCURRENCE('M4x10 Cap Screw:3',
'M4x10 Cap Screw:3','M4x10 Cap Screw:3',#11974,#11997,
'M4x10 Cap Screw:3');
#289=NEXT_ASSEMBLY_USAGE_OCCURRENCE('Roller support (1):1',
'Roller support (1):1','Roller support (1):1',#11974,#11989,
'Roller support (1):1');
#290=NEXT_ASSEMBLY_USAGE_OCCURRENCE('M6x18 mounting screw:4',
'M6x18 mounting screw:4','M6x18 mounting screw:4',#11974,#11990,
'M6x18 mounting screw:4');
#291=NEXT_ASSEMBLY_USAGE_OCCURRENCE('M6x18 mounting screw:5',
'M6x18 mounting screw:5','M6x18 mounting screw:5',#11974,#11990,
'M6x18 mounting screw:5');
#292=NEXT_ASSEMBLY_USAGE_OCCURRENCE('Dead axle (2):1','Dead axle (2):1',
'Dead axle (2):1',#11974,#11991,'Dead axle (2):1');
#293=NEXT_ASSEMBLY_USAGE_OCCURRENCE('Inner race spacer (5):1',
'Inner race spacer (5):1','Inner race spacer (5):1',#11974,#11992,
'Inner race spacer (5):1');
#294=NEXT_ASSEMBLY_USAGE_OCCURRENCE('Axle keeper (2):1',
'Axle keeper (2):1','Axle keeper (2):1',#11974,#11993,
'Axle keeper (2):1');
#295=NEXT_ASSEMBLY_USAGE_OCCURRENCE('M4x10 Cap Screw:4',
'M4x10 Cap Screw:4','M4x10 Cap Screw:4',#11974,#11997,
'M4x10 Cap Screw:4');
#296=NEXT_ASSEMBLY_USAGE_OCCURRENCE('Dead axle (3):1','Dead axle (3):1',
'Dead axle (3):1',#11974,#11994,'Dead axle (3):1');
#297=NEXT_ASSEMBLY_USAGE_OCCURRENCE('Inner race spacer (7):1',
'Inner race spacer (7):1','Inner race spacer (7):1',#11974,#11995,
'Inner race spacer (7):1');
#298=NEXT_ASSEMBLY_USAGE_OCCURRENCE('Axle keeper (3):1',
'Axle keeper (3):1','Axle keeper (3):1',#11974,#11996,
'Axle keeper (3):1');
#299=NEXT_ASSEMBLY_USAGE_OCCURRENCE('M4x10 Cap Screw:5',
'M4x10 Cap Screw:5','M4x10 Cap Screw:5',#11974,#11997,
'M4x10 Cap Screw:5');
#300=NEXT_ASSEMBLY_USAGE_OCCURRENCE('Indicator pedestal:1',
'Indicator pedestal:1','Indicator pedestal:1',#11974,#11998,
'Indicator pedestal:1');
#301=NEXT_ASSEMBLY_USAGE_OCCURRENCE('M5x14 Cap Screw:8',
'M5x14 Cap Screw:8','M5x14 Cap Screw:8',#11974,#11999,
'M5x14 Cap Screw:8');
#302=NEXT_ASSEMBLY_USAGE_OCCURRENCE('M5x14 Cap Screw:9',
'M5x14 Cap Screw:9','M5x14 Cap Screw:9',#11974,#11999,
'M5x14 Cap Screw:9');
#303=NEXT_ASSEMBLY_USAGE_OCCURRENCE('Indicator cross arm:1',
'Indicator cross arm:1','Indicator cross arm:1',#11974,#12000,
'Indicator cross arm:1');
#304=NEXT_ASSEMBLY_USAGE_OCCURRENCE('Socket Set Screw - M5x8:2',
'Socket Set Screw - M5x8:2','Socket Set Screw - M5x8:2',#11974,#12001,
'Socket Set Screw - M5x8:2');
#305=NEXT_ASSEMBLY_USAGE_OCCURRENCE('Socket Set Screw - M5x8:3',
'Socket Set Screw - M5x8:3','Socket Set Screw - M5x8:3',#11974,#12001,
'Socket Set Screw - M5x8:3');
#306=NEXT_ASSEMBLY_USAGE_OCCURRENCE('Indicator envelope:1',
'Indicator envelope:1','Indicator envelope:1',#11974,#12002,
'Indicator envelope:1');
#307=NEXT_ASSEMBLY_USAGE_OCCURRENCE('Indicator dial face:1',
'Indicator dial face:1','Indicator dial face:1',#11974,#12003,
'Indicator dial face:1');
#308=NEXT_ASSEMBLY_USAGE_OCCURRENCE('Dial pointer:1','Dial pointer:1',
'Dial pointer:1',#11974,#12004,'Dial pointer:1');
#309=NEXT_ASSEMBLY_USAGE_OCCURRENCE('Indicator probe:1',
'Indicator probe:1','Indicator probe:1',#11974,#12005,
'Indicator probe:1');
#310=NEXT_ASSEMBLY_USAGE_OCCURRENCE('Inner race spacer (2):1',
'Inner race spacer (2):1','Inner race spacer (2):1',#11974,#12006,
'Inner race spacer (2):1');
#311=NEXT_ASSEMBLY_USAGE_OCCURRENCE('Inner race spacer (6):1',
'Inner race spacer (6):1','Inner race spacer (6):1',#11974,#12007,
'Inner race spacer (6):1');
#312=NEXT_ASSEMBLY_USAGE_OCCURRENCE('Inner race spacer (4):1',
'Inner race spacer (4):1','Inner race spacer (4):1',#11974,#12008,
'Inner race spacer (4):1');
#313=NEXT_ASSEMBLY_USAGE_OCCURRENCE('Example shaft:1','Example shaft:1',
'Example shaft:1',#12009,#12010,'Example shaft:1');
#314=NEXT_ASSEMBLY_USAGE_OCCURRENCE('Inner ring:1','Inner ring:1',
'Inner ring:1',#12012,#12013,'Inner ring:1');
#315=NEXT_ASSEMBLY_USAGE_OCCURRENCE('Outer ring:1','Outer ring:1',
'Outer ring:1',#12012,#12014,'Outer ring:1');
#316=NEXT_ASSEMBLY_USAGE_OCCURRENCE('Balls:1','Balls:1','Balls:1',#12012,
#12015,'Balls:1');
#317=NEXT_ASSEMBLY_USAGE_OCCURRENCE('Cage:1','Cage:1','Cage:1',#12012,#12016,
'Cage:1');
#318=NEXT_ASSEMBLY_USAGE_OCCURRENCE('Seals 2RS:1','Seals 2RS:1',
'Seals 2RS:1',#12012,#12017,'Seals 2RS:1');
#319=NEXT_ASSEMBLY_USAGE_OCCURRENCE(
'Sealed Ball Bearing - 10 x 30 x 9 mm:2',
'Sealed Ball Bearing - 10 x 30 x 9 mm:2',
'Sealed Ball Bearing - 10 x 30 x 9 mm:2',#12011,#12012,
'Sealed Ball Bearing - 10 x 30 x 9 mm:2');
#320=NEXT_ASSEMBLY_USAGE_OCCURRENCE('Roller tread:1','Roller tread:1',
'Roller tread:1',#12011,#12018,'Roller tread:1');
#321=NEXT_ASSEMBLY_USAGE_OCCURRENCE('Bonded outer race retainer:1',
'Bonded outer race retainer:1','Bonded outer race retainer:1',#12011,#12019,
'Bonded outer race retainer:1');
#322=NEXT_ASSEMBLY_USAGE_OCCURRENCE('Bonded outer race retainer (1):1',
'Bonded outer race retainer (1):1','Bonded outer race retainer (1):1',#12011,
#12020,'Bonded outer race retainer (1):1');
#323=NEXT_ASSEMBLY_USAGE_OCCURRENCE('Frame and indicator:1',
'Frame and indicator:1','Frame and indicator:1',#11973,#11974,
'Frame and indicator:1');
#324=NEXT_ASSEMBLY_USAGE_OCCURRENCE('Support roller:1',
'Support roller:1','Support roller:1',#11973,#12011,'Support roller:1');
#325=NEXT_ASSEMBLY_USAGE_OCCURRENCE('Example shaft (1):1',
'Example shaft (1):1','Example shaft (1):1',#11973,#12009,
'Example shaft (1):1');
#326=NEXT_ASSEMBLY_USAGE_OCCURRENCE('Support roller:2',
'Support roller:2','Support roller:2',#11973,#12011,'Support roller:2');
#327=NEXT_ASSEMBLY_USAGE_OCCURRENCE('Support roller:3',
'Support roller:3','Support roller:3',#11973,#12011,'Support roller:3');
#328=NEXT_ASSEMBLY_USAGE_OCCURRENCE('Support roller:4',
'Support roller:4','Support roller:4',#11973,#12011,'Support roller:4');
#329=B_SPLINE_CURVE_WITH_KNOTS('',3,(#10633,#10634,#10635,#10636,#10637,
#10638,#10639,#10640,#10641,#10642),.UNSPECIFIED.,.F.,.F.,(4,2,2,2,4),(0.882019934661292,
0.890219855506043,0.970998038219416,1.05177622093279,1.05997614177754),
 .UNSPECIFIED.);
#330=B_SPLINE_CURVE_WITH_KNOTS('',3,(#10645,#10646,#10647,#10648,#10649,
#10650,#10651,#10652,#10653,#10654),.UNSPECIFIED.,.F.,.F.,(4,2,2,2,4),(0.234687909181681,
0.242887830026432,0.323666012739805,0.404444195453179,0.41264411629793),
 .UNSPECIFIED.);
#331=B_SPLINE_CURVE_WITH_KNOTS('',3,(#10669,#10670,#10671,#10672,#10673,
#10674,#10675,#10676,#10677,#10678,#10679,#10680,#10681,#10682),
 .UNSPECIFIED.,.F.,.F.,(4,2,2,2,2,2,4),(0.761877411255191,0.798325568640294,
0.878131747417165,0.957937926194035,1.03774410497091,1.11755028374778,1.15399844113288),
 .UNSPECIFIED.);
#332=B_SPLINE_CURVE_WITH_KNOTS('',3,(#10685,#10686,#10687,#10688,#10689,
#10690,#10691,#10692,#10693,#10694,#10695,#10696,#10697,#10698),
 .UNSPECIFIED.,.F.,.F.,(4,2,2,2,2,2,4),(0.123252127125832,0.159700284510937,
0.239506463287808,0.319312642064678,0.399118820841549,0.47892499961842,
0.515373157003523),.UNSPECIFIED.);
#333=B_SPLINE_CURVE_WITH_KNOTS('',3,(#10807,#10808,#10809,#10810,#10811,
#10812,#10813,#10814,#10815,#10816,#10817,#10818,#10819,#10820,#10821,#10822,
#10823,#10824),.UNSPECIFIED.,.F.,.F.,(4,2,2,2,2,2,2,2,4),(0.,0.151225950236217,
0.302451900472435,0.453664817813398,0.604877735154361,0.756090652495325,
0.907303569836288,1.05852952007251,1.20975547030872),.UNSPECIFIED.);
#334=B_SPLINE_CURVE_WITH_KNOTS('',3,(#10825,#10826,#10827,#10828,#10829,
#10830,#10831,#10832,#10833,#10834,#10835,#10836,#10837,#10838,#10839,#10840,
#10841,#10842),.UNSPECIFIED.,.F.,.F.,(4,2,2,2,2,2,2,2,4),(1.20975547030872,
1.36098142054494,1.51220737078116,1.66342028812212,1.81463320546308,1.96584612280405,
2.11705904014501,2.26828499038123,2.41951094061745),.UNSPECIFIED.);
#335=B_SPLINE_CURVE_WITH_KNOTS('',3,(#11118,#11119,#11120,#11121,#11122,
#11123,#11124,#11125,#11126,#11127,#11128,#11129,#11130,#11131,#11132,#11133,
#11134,#11135,#11136,#11137,#11138,#11139),.UNSPECIFIED.,.F.,.F.,(4,2,2,
2,2,2,2,2,2,2,4),(0.0473477652366656,0.126350602536658,0.189525903804987,
0.252701205073317,0.313298422430275,0.373895639787233,0.434492857144191,
0.495090074501149,0.558265375769478,0.621440677037807,0.7004435143378),
 .UNSPECIFIED.);
#336=B_SPLINE_CURVE_WITH_KNOTS('',3,(#11143,#11144,#11145,#11146,#11147,
#11148,#11149,#11150,#11151,#11152,#11153,#11154,#11155,#11156,#11157,#11158,
#11159,#11160,#11161,#11162,#11163,#11164),.UNSPECIFIED.,.F.,.F.,(4,2,2,
2,2,2,2,2,2,2,4),(0.0464897534940957,0.0852567806515119,0.170513561303024,
0.246687263103517,0.308657850341199,0.370628437578881,0.432599024816563,
0.494569612054245,0.570743313854739,0.656000094506251,0.694767121663666),
 .UNSPECIFIED.);
#337=B_SPLINE_CURVE_WITH_KNOTS('',3,(#11170,#11171,#11172,#11173,#11174,
#11175,#11176,#11177,#11178,#11179,#11180,#11181,#11182,#11183,#11184,#11185,
#11186,#11187,#11188,#11189,#11190,#11191),.UNSPECIFIED.,.F.,.F.,(4,2,2,
2,2,2,2,2,2,2,4),(0.0464897534940957,0.0852567806515118,0.170513561303024,
0.246687263103517,0.308657850341199,0.370628437578881,0.432599024816563,
0.494569612054245,0.570743313854738,0.65600009450625,0.694767121663666),
 .UNSPECIFIED.);
#338=B_SPLINE_CURVE_WITH_KNOTS('',3,(#11195,#11196,#11197,#11198,#11199,
#11200,#11201,#11202,#11203,#11204,#11205,#11206,#11207,#11208,#11209,#11210,
#11211,#11212,#11213,#11214,#11215,#11216),.UNSPECIFIED.,.F.,.F.,(4,2,2,
2,2,2,2,2,2,2,4),(0.0464897534940957,0.0852567806515119,0.170513561303024,
0.246687263103517,0.308657850341199,0.370628437578881,0.432599024816563,
0.494569612054245,0.570743313854739,0.656000094506251,0.694767121663666),
 .UNSPECIFIED.);
#339=B_SPLINE_CURVE_WITH_KNOTS('',3,(#11220,#11221,#11222,#11223,#11224,
#11225,#11226,#11227,#11228,#11229,#11230,#11231),.UNSPECIFIED.,.F.,.F.,
(4,2,2,2,2,4),(0.0464897534940957,0.0852567806515119,0.170513561303024,
0.246687263103517,0.308657850341199,0.370628437578881),.UNSPECIFIED.);
#340=B_SPLINE_CURVE_WITH_KNOTS('',3,(#11236,#11237,#11238,#11239,#11240,
#11241,#11242,#11243,#11244,#11245,#11246,#11247),.UNSPECIFIED.,.F.,.F.,
(4,2,2,2,2,4),(0.370628437578881,0.432599024816563,0.494569612054245,0.570743313854738,
0.65600009450625,0.694767121663666),.UNSPECIFIED.);
#341=B_SPLINE_CURVE_WITH_KNOTS('',3,(#11251,#11252,#11253,#11254,#11255,
#11256,#11257,#11258,#11259,#11260,#11261,#11262,#11263,#11264,#11265,#11266,
#11267,#11268,#11269,#11270,#11271,#11272),.UNSPECIFIED.,.F.,.F.,(4,2,2,
2,2,2,2,2,2,2,4),(0.0464897534940957,0.0852567806515121,0.170513561303024,
0.246687263103518,0.308657850341199,0.370628437578881,0.432599024816563,
0.494569612054245,0.570743313854738,0.65600009450625,0.694767121663666),
 .UNSPECIFIED.);
#342=B_SPLINE_CURVE_WITH_KNOTS('',3,(#11276,#11277,#11278,#11279,#11280,
#11281,#11282,#11283,#11284,#11285,#11286,#11287,#11288,#11289,#11290,#11291,
#11292,#11293,#11294,#11295,#11296,#11297),.UNSPECIFIED.,.F.,.F.,(4,2,2,
2,2,2,2,2,2,2,4),(0.0464897534940957,0.0852567806515119,0.170513561303024,
0.246687263103517,0.308657850341199,0.370628437578881,0.432599024816563,
0.494569612054245,0.570743313854738,0.65600009450625,0.694767121663667),
 .UNSPECIFIED.);
#343=B_SPLINE_CURVE_WITH_KNOTS('',3,(#11301,#11302,#11303,#11304,#11305,
#11306,#11307,#11308,#11309,#11310,#11311,#11312,#11313,#11314,#11315,#11316,
#11317,#11318,#11319,#11320,#11321,#11322),.UNSPECIFIED.,.F.,.F.,(4,2,2,
2,2,2,2,2,2,2,4),(0.0464897534940957,0.0852567806515119,0.170513561303024,
0.246687263103517,0.308657850341199,0.370628437578881,0.432599024816563,
0.494569612054245,0.570743313854738,0.65600009450625,0.694767121663666),
 .UNSPECIFIED.);
#344=B_SPLINE_CURVE_WITH_KNOTS('',3,(#11326,#11327,#11328,#11329,#11330,
#11331,#11332,#11333,#11334,#11335,#11336,#11337,#11338,#11339,#11340,#11341,
#11342,#11343,#11344,#11345,#11346,#11347),.UNSPECIFIED.,.F.,.F.,(4,2,2,
2,2,2,2,2,2,2,4),(0.0464897534940957,0.0852567806515119,0.170513561303024,
0.246687263103517,0.308657850341199,0.370628437578881,0.432599024816563,
0.494569612054245,0.570743313854739,0.656000094506251,0.694767121663667),
 .UNSPECIFIED.);
#345=B_SPLINE_CURVE_WITH_KNOTS('',3,(#11355,#11356,#11357,#11358,#11359,
#11360,#11361,#11362,#11363,#11364,#11365,#11366,#11367,#11368,#11369,#11370,
#11371,#11372,#11373,#11374,#11375,#11376),.UNSPECIFIED.,.F.,.F.,(4,2,2,
2,2,2,2,2,2,2,4),(0.0473477652366656,0.126350602536658,0.189525903804987,
0.252701205073316,0.313298422430274,0.373895639787232,0.434492857144191,
0.495090074501149,0.558265375769478,0.621440677037807,0.7004435143378),
 .UNSPECIFIED.);
#346=B_SPLINE_CURVE_WITH_KNOTS('',3,(#11384,#11385,#11386,#11387,#11388,
#11389,#11390,#11391,#11392,#11393,#11394,#11395,#11396,#11397,#11398,#11399,
#11400,#11401,#11402,#11403,#11404,#11405),.UNSPECIFIED.,.F.,.F.,(4,2,2,
2,2,2,2,2,2,2,4),(0.0473477652366656,0.126350602536658,0.189525903804987,
0.252701205073317,0.313298422430275,0.373895639787233,0.434492857144191,
0.495090074501149,0.558265375769478,0.621440677037807,0.7004435143378),
 .UNSPECIFIED.);
#347=B_SPLINE_CURVE_WITH_KNOTS('',3,(#11414,#11415,#11416,#11417,#11418,
#11419,#11420,#11421,#11422,#11423,#11424,#11425),.UNSPECIFIED.,.F.,.F.,
(4,2,2,2,2,4),(0.0473477652366656,0.126350602536658,0.189525903804987,0.252701205073316,
0.313298422430275,0.373895639787233),.UNSPECIFIED.);
#348=B_SPLINE_CURVE_WITH_KNOTS('',3,(#11427,#11428,#11429,#11430,#11431,
#11432,#11433,#11434,#11435,#11436,#11437,#11438),.UNSPECIFIED.,.F.,.F.,
(4,2,2,2,2,4),(0.373895639787233,0.434492857144191,0.495090074501149,0.558265375769478,
0.621440677037807,0.7004435143378),.UNSPECIFIED.);
#349=B_SPLINE_CURVE_WITH_KNOTS('',3,(#11445,#11446,#11447,#11448,#11449,
#11450,#11451,#11452,#11453,#11454,#11455,#11456,#11457,#11458,#11459,#11460,
#11461,#11462,#11463,#11464,#11465,#11466),.UNSPECIFIED.,.F.,.F.,(4,2,2,
2,2,2,2,2,2,2,4),(0.0473477652366656,0.126350602536658,0.189525903804987,
0.252701205073316,0.313298422430275,0.373895639787233,0.434492857144191,
0.495090074501149,0.558265375769478,0.621440677037807,0.7004435143378),
 .UNSPECIFIED.);
#350=B_SPLINE_CURVE_WITH_KNOTS('',3,(#11474,#11475,#11476,#11477,#11478,
#11479,#11480,#11481,#11482,#11483,#11484,#11485,#11486,#11487,#11488,#11489,
#11490,#11491,#11492,#11493,#11494,#11495),.UNSPECIFIED.,.F.,.F.,(4,2,2,
2,2,2,2,2,2,2,4),(0.0473477652366656,0.126350602536658,0.189525903804987,
0.252701205073317,0.313298422430275,0.373895639787233,0.434492857144191,
0.495090074501149,0.558265375769478,0.621440677037807,0.7004435143378),
 .UNSPECIFIED.);
#351=B_SPLINE_CURVE_WITH_KNOTS('',3,(#11503,#11504,#11505,#11506,#11507,
#11508,#11509,#11510,#11511,#11512,#11513,#11514,#11515,#11516,#11517,#11518,
#11519,#11520,#11521,#11522,#11523,#11524),.UNSPECIFIED.,.F.,.F.,(4,2,2,
2,2,2,2,2,2,2,4),(0.0473477652366656,0.126350602536658,0.189525903804987,
0.252701205073316,0.313298422430275,0.373895639787233,0.434492857144191,
0.495090074501149,0.558265375769478,0.621440677037807,0.7004435143378),
 .UNSPECIFIED.);
#352=B_SPLINE_CURVE_WITH_KNOTS('',3,(#11533,#11534,#11535,#11536,#11537,
#11538,#11539,#11540,#11541,#11542,#11543,#11544,#11545,#11546,#11547,#11548,
#11549,#11550,#11551,#11552,#11553,#11554),.UNSPECIFIED.,.F.,.F.,(4,2,2,
2,2,2,2,2,2,2,4),(0.0473477652366656,0.126350602536658,0.189525903804987,
0.252701205073317,0.313298422430275,0.373895639787233,0.434492857144191,
0.495090074501149,0.558265375769478,0.621440677037807,0.7004435143378),
 .UNSPECIFIED.);
#353=ORIENTED_CLOSED_SHELL('',*,#6221,.F.);
#354=ORIENTED_CLOSED_SHELL('',*,#6229,.F.);
#355=ORIENTED_CLOSED_SHELL('',*,#6232,.F.);
#356=BREP_WITH_VOIDS('Body1',#6222,(#353));
#357=BREP_WITH_VOIDS('Body1',#6230,(#354));
#358=BREP_WITH_VOIDS('Body1',#6233,(#355));
#359=CONICAL_SURFACE('',#6851,0.275,0.785398163397449);
#360=CONICAL_SURFACE('',#7011,0.475,0.785398163397449);
#361=CONICAL_SURFACE('',#7015,0.485,0.785398163397448);
#362=CONICAL_SURFACE('',#7019,0.31,0.463647609000806);
#363=CONICAL_SURFACE('',#7099,0.325,0.785398163397448);
#364=CONICAL_SURFACE('',#7103,0.335,0.785398163397448);
#365=CONICAL_SURFACE('',#7107,0.21,0.463647609000806);
#366=CONICAL_SURFACE('',#7140,0.4,0.785398163397448);
#367=CONICAL_SURFACE('',#7144,0.41,0.785398163397448);
#368=CONICAL_SURFACE('',#7148,0.26,0.463647609000806);
#369=CONICAL_SURFACE('',#7188,0.235,0.785398163397448);
#370=CONICAL_SURFACE('',#7192,0.2125,0.785398163397448);
#371=CONICAL_SURFACE('',#7334,0.53,0.785398163397448);
#372=CONICAL_SURFACE('',#7341,0.53,0.785398163397448);
#373=CONICAL_SURFACE('',#7354,1.47,0.785398163397449);
#374=CONICAL_SURFACE('',#7358,1.47,0.785398163397449);
#375=ELLIPSE('',#6840,0.299389011154384,0.2117);
#376=ELLIPSE('',#6844,0.299389011154384,0.2117);
#377=SHAPE_REPRESENTATION_RELATIONSHIP('SRR','None',#11926,#420);
#378=SHAPE_REPRESENTATION_RELATIONSHIP('SRR','None',#11927,#421);
#379=SHAPE_REPRESENTATION_RELATIONSHIP('SRR','None',#11928,#422);
#380=SHAPE_REPRESENTATION_RELATIONSHIP('SRR','None',#11929,#423);
#381=SHAPE_REPRESENTATION_RELATIONSHIP('SRR','None',#11930,#424);
#382=SHAPE_REPRESENTATION_RELATIONSHIP('SRR','None',#11931,#425);
#383=SHAPE_REPRESENTATION_RELATIONSHIP('SRR','None',#11932,#426);
#384=SHAPE_REPRESENTATION_RELATIONSHIP('SRR','None',#11933,#427);
#385=SHAPE_REPRESENTATION_RELATIONSHIP('SRR','None',#11934,#428);
#386=SHAPE_REPRESENTATION_RELATIONSHIP('SRR','None',#11935,#429);
#387=SHAPE_REPRESENTATION_RELATIONSHIP('SRR','None',#11936,#430);
#388=SHAPE_REPRESENTATION_RELATIONSHIP('SRR','None',#11937,#431);
#389=SHAPE_REPRESENTATION_RELATIONSHIP('SRR','None',#11938,#432);
#390=SHAPE_REPRESENTATION_RELATIONSHIP('SRR','None',#11939,#433);
#391=SHAPE_REPRESENTATION_RELATIONSHIP('SRR','None',#11940,#434);
#392=SHAPE_REPRESENTATION_RELATIONSHIP('SRR','None',#11941,#435);
#393=SHAPE_REPRESENTATION_RELATIONSHIP('SRR','None',#11942,#436);
#394=SHAPE_REPRESENTATION_RELATIONSHIP('SRR','None',#11943,#437);
#395=SHAPE_REPRESENTATION_RELATIONSHIP('SRR','None',#11944,#438);
#396=SHAPE_REPRESENTATION_RELATIONSHIP('SRR','None',#11945,#439);
#397=SHAPE_REPRESENTATION_RELATIONSHIP('SRR','None',#11946,#440);
#398=SHAPE_REPRESENTATION_RELATIONSHIP('SRR','None',#11947,#441);
#399=SHAPE_REPRESENTATION_RELATIONSHIP('SRR','None',#11948,#442);
#400=SHAPE_REPRESENTATION_RELATIONSHIP('SRR','None',#11949,#443);
#401=SHAPE_REPRESENTATION_RELATIONSHIP('SRR','None',#11950,#444);
#402=SHAPE_REPRESENTATION_RELATIONSHIP('SRR','None',#11951,#445);
#403=SHAPE_REPRESENTATION_RELATIONSHIP('SRR','None',#11952,#446);
#404=SHAPE_REPRESENTATION_RELATIONSHIP('SRR','None',#11953,#447);
#405=SHAPE_REPRESENTATION_RELATIONSHIP('SRR','None',#11954,#448);
#406=SHAPE_REPRESENTATION_RELATIONSHIP('SRR','None',#11955,#449);
#407=SHAPE_REPRESENTATION_RELATIONSHIP('SRR','None',#11956,#450);
#408=SHAPE_REPRESENTATION_RELATIONSHIP('SRR','None',#11957,#451);
#409=SHAPE_REPRESENTATION_RELATIONSHIP('SRR','None',#11958,#452);
#410=SHAPE_REPRESENTATION_RELATIONSHIP('SRR','None',#11959,#453);
#411=SHAPE_REPRESENTATION_RELATIONSHIP('SRR','None',#11961,#454);
#412=SHAPE_REPRESENTATION_RELATIONSHIP('SRR','None',#11964,#455);
#413=SHAPE_REPRESENTATION_RELATIONSHIP('SRR','None',#11965,#456);
#414=SHAPE_REPRESENTATION_RELATIONSHIP('SRR','None',#11966,#457);
#415=SHAPE_REPRESENTATION_RELATIONSHIP('SRR','None',#11967,#458);
#416=SHAPE_REPRESENTATION_RELATIONSHIP('SRR','None',#11968,#459);
#417=SHAPE_REPRESENTATION_RELATIONSHIP('SRR','None',#11969,#460);
#418=SHAPE_REPRESENTATION_RELATIONSHIP('SRR','None',#11970,#461);
#419=SHAPE_REPRESENTATION_RELATIONSHIP('SRR','None',#11971,#462);
#420=ADVANCED_BREP_SHAPE_REPRESENTATION('',(#514),#11702);
#421=ADVANCED_BREP_SHAPE_REPRESENTATION('',(#515),#11703);
#422=ADVANCED_BREP_SHAPE_REPRESENTATION('',(#516),#11704);
#423=ADVANCED_BREP_SHAPE_REPRESENTATION('',(#517),#11705);
#424=ADVANCED_BREP_SHAPE_REPRESENTATION('',(#518),#11706);
#425=ADVANCED_BREP_SHAPE_REPRESENTATION('',(#519),#11707);
#426=ADVANCED_BREP_SHAPE_REPRESENTATION('',(#520),#11708);
#427=ADVANCED_BREP_SHAPE_REPRESENTATION('',(#521),#11709);
#428=ADVANCED_BREP_SHAPE_REPRESENTATION('',(#522),#11710);
#429=ADVANCED_BREP_SHAPE_REPRESENTATION('',(#523),#11711);
#430=ADVANCED_BREP_SHAPE_REPRESENTATION('',(#524),#11712);
#431=ADVANCED_BREP_SHAPE_REPRESENTATION('',(#525),#11713);
#432=ADVANCED_BREP_SHAPE_REPRESENTATION('',(#526),#11714);
#433=ADVANCED_BREP_SHAPE_REPRESENTATION('',(#527),#11715);
#434=ADVANCED_BREP_SHAPE_REPRESENTATION('',(#528),#11716);
#435=ADVANCED_BREP_SHAPE_REPRESENTATION('',(#356),#11717);
#436=ADVANCED_BREP_SHAPE_REPRESENTATION('',(#529),#11718);
#437=ADVANCED_BREP_SHAPE_REPRESENTATION('',(#530),#11719);
#438=ADVANCED_BREP_SHAPE_REPRESENTATION('',(#531),#11720);
#439=ADVANCED_BREP_SHAPE_REPRESENTATION('',(#532),#11721);
#440=ADVANCED_BREP_SHAPE_REPRESENTATION('',(#533),#11722);
#441=ADVANCED_BREP_SHAPE_REPRESENTATION('',(#534),#11723);
#442=ADVANCED_BREP_SHAPE_REPRESENTATION('',(#357),#11724);
#443=ADVANCED_BREP_SHAPE_REPRESENTATION('',(#535),#11725);
#444=ADVANCED_BREP_SHAPE_REPRESENTATION('',(#358),#11726);
#445=ADVANCED_BREP_SHAPE_REPRESENTATION('',(#536),#11727);
#446=ADVANCED_BREP_SHAPE_REPRESENTATION('',(#537),#11728);
#447=ADVANCED_BREP_SHAPE_REPRESENTATION('',(#538),#11729);
#448=ADVANCED_BREP_SHAPE_REPRESENTATION('',(#539),#11730);
#449=ADVANCED_BREP_SHAPE_REPRESENTATION('',(#540),#11731);
#450=ADVANCED_BREP_SHAPE_REPRESENTATION('',(#541),#11732);
#451=ADVANCED_BREP_SHAPE_REPRESENTATION('',(#542),#11733);
#452=ADVANCED_BREP_SHAPE_REPRESENTATION('',(#543),#11734);
#453=ADVANCED_BREP_SHAPE_REPRESENTATION('',(#544),#11735);
#454=ADVANCED_BREP_SHAPE_REPRESENTATION('',(#545),#11737);
#455=ADVANCED_BREP_SHAPE_REPRESENTATION('',(#546),#11740);
#456=ADVANCED_BREP_SHAPE_REPRESENTATION('',(#547),#11741);
#457=ADVANCED_BREP_SHAPE_REPRESENTATION('',(#548,#549,#550,#551,#552,#553,
#554,#555),#11742);
#458=ADVANCED_BREP_SHAPE_REPRESENTATION('',(#556),#11743);
#459=ADVANCED_BREP_SHAPE_REPRESENTATION('',(#557,#558),#11744);
#460=ADVANCED_BREP_SHAPE_REPRESENTATION('',(#559),#11745);
#461=ADVANCED_BREP_SHAPE_REPRESENTATION('',(#560),#11746);
#462=ADVANCED_BREP_SHAPE_REPRESENTATION('',(#561),#11747);
#463=STYLED_ITEM('',(#12169),#514);
#464=STYLED_ITEM('',(#12169),#515);
#465=STYLED_ITEM('',(#12169),#516);
#466=STYLED_ITEM('',(#12170),#517);
#467=STYLED_ITEM('',(#12171),#518);
#468=STYLED_ITEM('',(#12171),#519);
#469=STYLED_ITEM('',(#12169),#520);
#470=STYLED_ITEM('',(#12169),#521);
#471=STYLED_ITEM('',(#12170),#522);
#472=STYLED_ITEM('',(#12170),#523);
#473=STYLED_ITEM('',(#12169),#524);
#474=STYLED_ITEM('',(#12169),#525);
#475=STYLED_ITEM('',(#12170),#526);
#476=STYLED_ITEM('',(#12169),#527);
#477=STYLED_ITEM('',(#12169),#528);
#478=STYLED_ITEM('',(#12172),#356);
#479=STYLED_ITEM('',(#12169),#529);
#480=STYLED_ITEM('',(#12170),#530);
#481=STYLED_ITEM('',(#12169),#531);
#482=STYLED_ITEM('',(#12169),#532);
#483=STYLED_ITEM('',(#12170),#533);
#484=STYLED_ITEM('',(#12169),#534);
#485=STYLED_ITEM('',(#12172),#357);
#486=STYLED_ITEM('',(#12169),#535);
#487=STYLED_ITEM('',(#12172),#358);
#488=STYLED_ITEM('',(#12169),#536);
#489=STYLED_ITEM('',(#12172),#537);
#490=STYLED_ITEM('',(#12169),#538);
#491=STYLED_ITEM('',(#12169),#539);
#492=STYLED_ITEM('',(#12169),#540);
#493=STYLED_ITEM('',(#12169),#541);
#494=STYLED_ITEM('',(#12170),#542);
#495=STYLED_ITEM('',(#12170),#543);
#496=STYLED_ITEM('',(#12170),#544);
#497=STYLED_ITEM('',(#12170),#545);
#498=STYLED_ITEM('',(#12170),#546);
#499=STYLED_ITEM('',(#12170),#547);
#500=STYLED_ITEM('',(#12170),#548);
#501=STYLED_ITEM('',(#12170),#549);
#502=STYLED_ITEM('',(#12170),#550);
#503=STYLED_ITEM('',(#12170),#551);
#504=STYLED_ITEM('',(#12170),#552);
#505=STYLED_ITEM('',(#12170),#553);
#506=STYLED_ITEM('',(#12170),#554);
#507=STYLED_ITEM('',(#12170),#555);
#508=STYLED_ITEM('',(#12169),#556);
#509=STYLED_ITEM('',(#12169),#557);
#510=STYLED_ITEM('',(#12169),#558);
#511=STYLED_ITEM('',(#12169),#559);
#512=STYLED_ITEM('',(#12169),#560);
#513=STYLED_ITEM('',(#12169),#561);
#514=MANIFOLD_SOLID_BREP('Body1',#6206);
#515=MANIFOLD_SOLID_BREP('Body1',#6207);
#516=MANIFOLD_SOLID_BREP('Body1',#6208);
#517=MANIFOLD_SOLID_BREP('Body1',#6209);
#518=MANIFOLD_SOLID_BREP('Body1',#6210);
#519=MANIFOLD_SOLID_BREP('Body1',#6211);
#520=MANIFOLD_SOLID_BREP('Body1',#6212);
#521=MANIFOLD_SOLID_BREP('Body1',#6213);
#522=MANIFOLD_SOLID_BREP('Body1',#6214);
#523=MANIFOLD_SOLID_BREP('Body1',#6215);
#524=MANIFOLD_SOLID_BREP('Body1',#6216);
#525=MANIFOLD_SOLID_BREP('Body1',#6217);
#526=MANIFOLD_SOLID_BREP('Body1',#6218);
#527=MANIFOLD_SOLID_BREP('Body1',#6219);
#528=MANIFOLD_SOLID_BREP('Body1',#6220);
#529=MANIFOLD_SOLID_BREP('Body1',#6223);
#530=MANIFOLD_SOLID_BREP('Body1',#6224);
#531=MANIFOLD_SOLID_BREP('Body1',#6225);
#532=MANIFOLD_SOLID_BREP('Body1',#6226);
#533=MANIFOLD_SOLID_BREP('Body1',#6227);
#534=MANIFOLD_SOLID_BREP('Body1',#6228);
#535=MANIFOLD_SOLID_BREP('Body1',#6231);
#536=MANIFOLD_SOLID_BREP('Body1',#6234);
#537=MANIFOLD_SOLID_BREP('Body1',#6235);
#538=MANIFOLD_SOLID_BREP('Body1',#6236);
#539=MANIFOLD_SOLID_BREP('Body1',#6237);
#540=MANIFOLD_SOLID_BREP('Body1',#6238);
#541=MANIFOLD_SOLID_BREP('Body1',#6239);
#542=MANIFOLD_SOLID_BREP('Body1',#6240);
#543=MANIFOLD_SOLID_BREP('Body1',#6241);
#544=MANIFOLD_SOLID_BREP('Body1',#6242);
#545=MANIFOLD_SOLID_BREP('Body1',#6243);
#546=MANIFOLD_SOLID_BREP('Body1',#6244);
#547=MANIFOLD_SOLID_BREP('Body1',#6245);
#548=MANIFOLD_SOLID_BREP('Body1',#6246);
#549=MANIFOLD_SOLID_BREP('Body2',#6247);
#550=MANIFOLD_SOLID_BREP('Body3',#6248);
#551=MANIFOLD_SOLID_BREP('Body4',#6249);
#552=MANIFOLD_SOLID_BREP('Body5',#6250);
#553=MANIFOLD_SOLID_BREP('Body6',#6251);
#554=MANIFOLD_SOLID_BREP('Body7',#6252);
#555=MANIFOLD_SOLID_BREP('Body8',#6253);
#556=MANIFOLD_SOLID_BREP('Continuous crown cage',#6254);
#557=MANIFOLD_SOLID_BREP('Body1',#6255);
#558=MANIFOLD_SOLID_BREP('Body2',#6256);
#559=MANIFOLD_SOLID_BREP('Body1',#6257);
#560=MANIFOLD_SOLID_BREP('Body1',#6258);
#561=MANIFOLD_SOLID_BREP('Body1',#6259);
#562=FACE_BOUND('',#1452,.T.);
#563=FACE_BOUND('',#1454,.T.);
#564=FACE_BOUND('',#1472,.T.);
#565=FACE_BOUND('',#1473,.T.);
#566=FACE_BOUND('',#1474,.T.);
#567=FACE_BOUND('',#1475,.T.);
#568=FACE_BOUND('',#1476,.T.);
#569=FACE_BOUND('',#1477,.T.);
#570=FACE_BOUND('',#1478,.T.);
#571=FACE_BOUND('',#1479,.T.);
#572=FACE_BOUND('',#1480,.T.);
#573=FACE_BOUND('',#1481,.T.);
#574=FACE_BOUND('',#1482,.T.);
#575=FACE_BOUND('',#1483,.T.);
#576=FACE_BOUND('',#1485,.T.);
#577=FACE_BOUND('',#1486,.T.);
#578=FACE_BOUND('',#1487,.T.);
#579=FACE_BOUND('',#1488,.T.);
#580=FACE_BOUND('',#1489,.T.);
#581=FACE_BOUND('',#1490,.T.);
#582=FACE_BOUND('',#1491,.T.);
#583=FACE_BOUND('',#1492,.T.);
#584=FACE_BOUND('',#1493,.T.);
#585=FACE_BOUND('',#1494,.T.);
#586=FACE_BOUND('',#1495,.T.);
#587=FACE_BOUND('',#1496,.T.);
#588=FACE_BOUND('',#1500,.T.);
#589=FACE_BOUND('',#1515,.T.);
#590=FACE_BOUND('',#1518,.T.);
#591=FACE_BOUND('',#1535,.T.);
#592=FACE_BOUND('',#1536,.T.);
#593=FACE_BOUND('',#1541,.T.);
#594=FACE_BOUND('',#1542,.T.);
#595=FACE_BOUND('',#1546,.T.);
#596=FACE_BOUND('',#1547,.T.);
#597=FACE_BOUND('',#1551,.T.);
#598=FACE_BOUND('',#1552,.T.);
#599=FACE_BOUND('',#1556,.T.);
#600=FACE_BOUND('',#1561,.T.);
#601=FACE_BOUND('',#1565,.T.);
#602=FACE_BOUND('',#1567,.T.);
#603=FACE_BOUND('',#1571,.T.);
#604=FACE_BOUND('',#1573,.T.);
#605=FACE_BOUND('',#1577,.T.);
#606=FACE_BOUND('',#1579,.T.);
#607=FACE_BOUND('',#1583,.T.);
#608=FACE_BOUND('',#1588,.T.);
#609=FACE_BOUND('',#1592,.T.);
#610=FACE_BOUND('',#1594,.T.);
#611=FACE_BOUND('',#1598,.T.);
#612=FACE_BOUND('',#1600,.T.);
#613=FACE_BOUND('',#1605,.T.);
#614=FACE_BOUND('',#1606,.T.);
#615=FACE_BOUND('',#1611,.T.);
#616=FACE_BOUND('',#1612,.T.);
#617=FACE_BOUND('',#1616,.T.);
#618=FACE_BOUND('',#1617,.T.);
#619=FACE_BOUND('',#1621,.T.);
#620=FACE_BOUND('',#1622,.T.);
#621=FACE_BOUND('',#1637,.T.);
#622=FACE_BOUND('',#1643,.T.);
#623=FACE_BOUND('',#1648,.T.);
#624=FACE_BOUND('',#1652,.T.);
#625=FACE_BOUND('',#1654,.T.);
#626=FACE_BOUND('',#1658,.T.);
#627=FACE_BOUND('',#1660,.T.);
#628=FACE_BOUND('',#1664,.T.);
#629=FACE_BOUND('',#1669,.T.);
#630=FACE_BOUND('',#1673,.T.);
#631=FACE_BOUND('',#1675,.T.);
#632=FACE_BOUND('',#1679,.T.);
#633=FACE_BOUND('',#1681,.T.);
#634=FACE_BOUND('',#1696,.T.);
#635=FACE_BOUND('',#1708,.T.);
#636=FACE_BOUND('',#1709,.T.);
#637=FACE_BOUND('',#1710,.T.);
#638=FACE_BOUND('',#1712,.T.);
#639=FACE_BOUND('',#1713,.T.);
#640=FACE_BOUND('',#1728,.T.);
#641=FACE_BOUND('',#1738,.T.);
#642=FACE_BOUND('',#1740,.T.);
#643=FACE_BOUND('',#1742,.T.);
#644=FACE_BOUND('',#1743,.T.);
#645=FACE_BOUND('',#1748,.T.);
#646=FACE_BOUND('',#1749,.T.);
#647=FACE_BOUND('',#1751,.T.);
#648=FACE_BOUND('',#1752,.T.);
#649=FACE_BOUND('',#1761,.T.);
#650=FACE_BOUND('',#1770,.T.);
#651=FACE_BOUND('',#1772,.T.);
#652=FACE_BOUND('',#1789,.T.);
#653=FACE_BOUND('',#1791,.T.);
#654=FACE_BOUND('',#1795,.T.);
#655=FACE_BOUND('',#1797,.T.);
#656=FACE_BOUND('',#1801,.T.);
#657=FACE_BOUND('',#1803,.T.);
#658=FACE_BOUND('',#1812,.T.);
#659=FACE_BOUND('',#1815,.T.);
#660=FACE_BOUND('',#1820,.T.);
#661=FACE_BOUND('',#1825,.T.);
#662=FACE_BOUND('',#1853,.T.);
#663=FACE_BOUND('',#1856,.T.);
#664=FACE_BOUND('',#1859,.T.);
#665=FACE_BOUND('',#1862,.T.);
#666=FACE_BOUND('',#1865,.T.);
#667=FACE_BOUND('',#1870,.T.);
#668=FACE_BOUND('',#1872,.T.);
#669=FACE_BOUND('',#1876,.T.);
#670=FACE_BOUND('',#1878,.T.);
#671=FACE_BOUND('',#1882,.T.);
#672=FACE_BOUND('',#1884,.T.);
#673=CIRCLE('',#6774,0.21);
#674=CIRCLE('',#6775,0.21);
#675=CIRCLE('',#6788,0.21);
#676=CIRCLE('',#6789,0.21);
#677=CIRCLE('',#6791,0.21);
#678=CIRCLE('',#6792,0.21);
#679=CIRCLE('',#6794,0.25);
#680=CIRCLE('',#6795,0.25);
#681=CIRCLE('',#6797,0.25);
#682=CIRCLE('',#6798,0.25);
#683=CIRCLE('',#6800,0.25);
#684=CIRCLE('',#6801,0.25);
#685=CIRCLE('',#6803,0.25);
#686=CIRCLE('',#6804,0.25);
#687=CIRCLE('',#6806,0.275);
#688=CIRCLE('',#6807,0.275);
#689=CIRCLE('',#6809,0.275);
#690=CIRCLE('',#6810,0.275);
#691=CIRCLE('',#6812,0.275);
#692=CIRCLE('',#6813,0.275);
#693=CIRCLE('',#6815,0.275);
#694=CIRCLE('',#6816,0.275);
#695=CIRCLE('',#6818,0.275);
#696=CIRCLE('',#6819,0.275);
#697=CIRCLE('',#6821,0.275);
#698=CIRCLE('',#6822,0.275);
#699=CIRCLE('',#6833,0.2117);
#700=CIRCLE('',#6842,0.2117);
#701=CIRCLE('',#6843,0.2117);
#702=CIRCLE('',#6845,0.2117);
#703=CIRCLE('',#6852,0.285);
#704=CIRCLE('',#6853,0.265);
#705=CIRCLE('',#6855,0.265);
#706=CIRCLE('',#6857,0.5);
#707=CIRCLE('',#6859,0.5);
#708=CIRCLE('',#6877,0.33);
#709=CIRCLE('',#6878,0.33);
#710=CIRCLE('',#6880,0.33);
#711=CIRCLE('',#6881,0.33);
#712=CIRCLE('',#6883,1.1);
#713=CIRCLE('',#6884,1.1);
#714=CIRCLE('',#6886,0.5);
#715=CIRCLE('',#6887,0.5);
#716=CIRCLE('',#6890,0.5);
#717=CIRCLE('',#6892,0.5);
#718=CIRCLE('',#6902,0.165);
#719=CIRCLE('',#6903,0.165);
#720=CIRCLE('',#6906,0.8);
#721=CIRCLE('',#6907,0.5);
#722=CIRCLE('',#6909,0.8);
#723=CIRCLE('',#6912,0.5);
#724=CIRCLE('',#6916,0.505);
#725=CIRCLE('',#6917,0.505);
#726=CIRCLE('',#6919,0.7);
#727=CIRCLE('',#6920,0.7);
#728=CIRCLE('',#6925,0.505);
#729=CIRCLE('',#6926,0.505);
#730=CIRCLE('',#6928,0.7);
#731=CIRCLE('',#6929,0.7);
#732=CIRCLE('',#6934,0.225);
#733=CIRCLE('',#6935,0.225);
#734=CIRCLE('',#6937,0.8);
#735=CIRCLE('',#6938,0.8);
#736=CIRCLE('',#6943,0.165);
#737=CIRCLE('',#6944,0.165);
#738=CIRCLE('',#6947,0.8);
#739=CIRCLE('',#6948,0.5);
#740=CIRCLE('',#6950,0.8);
#741=CIRCLE('',#6953,0.5);
#742=CIRCLE('',#6957,0.505);
#743=CIRCLE('',#6958,0.505);
#744=CIRCLE('',#6960,0.7);
#745=CIRCLE('',#6961,0.7);
#746=CIRCLE('',#6966,0.225);
#747=CIRCLE('',#6967,0.225);
#748=CIRCLE('',#6969,0.8);
#749=CIRCLE('',#6970,0.8);
#750=CIRCLE('',#6975,0.33);
#751=CIRCLE('',#6976,0.33);
#752=CIRCLE('',#6978,0.33);
#753=CIRCLE('',#6979,0.33);
#754=CIRCLE('',#6981,1.1);
#755=CIRCLE('',#6982,1.1);
#756=CIRCLE('',#6984,0.5);
#757=CIRCLE('',#6985,0.5);
#758=CIRCLE('',#6988,0.5);
#759=CIRCLE('',#6990,0.5);
#760=CIRCLE('',#7008,0.2942);
#761=CIRCLE('',#7010,0.45);
#762=CIRCLE('',#7012,0.5);
#763=CIRCLE('',#7014,0.5);
#764=CIRCLE('',#7016,0.47);
#765=CIRCLE('',#7018,0.32);
#766=CIRCLE('',#7020,0.2942);
#767=CIRCLE('',#7024,0.165);
#768=CIRCLE('',#7025,0.165);
#769=CIRCLE('',#7028,0.8);
#770=CIRCLE('',#7029,0.5);
#771=CIRCLE('',#7031,0.8);
#772=CIRCLE('',#7034,0.5);
#773=CIRCLE('',#7038,0.505);
#774=CIRCLE('',#7039,0.505);
#775=CIRCLE('',#7041,0.7);
#776=CIRCLE('',#7042,0.7);
#777=CIRCLE('',#7047,0.225);
#778=CIRCLE('',#7048,0.225);
#779=CIRCLE('',#7050,0.8);
#780=CIRCLE('',#7051,0.8);
#781=CIRCLE('',#7056,0.165);
#782=CIRCLE('',#7057,0.165);
#783=CIRCLE('',#7060,0.8);
#784=CIRCLE('',#7061,0.5);
#785=CIRCLE('',#7063,0.8);
#786=CIRCLE('',#7066,0.5);
#787=CIRCLE('',#7070,0.505);
#788=CIRCLE('',#7071,0.505);
#789=CIRCLE('',#7073,0.7);
#790=CIRCLE('',#7074,0.7);
#791=CIRCLE('',#7079,0.225);
#792=CIRCLE('',#7080,0.225);
#793=CIRCLE('',#7082,0.8);
#794=CIRCLE('',#7083,0.8);
#795=CIRCLE('',#7096,0.1954);
#796=CIRCLE('',#7098,0.3);
#797=CIRCLE('',#7100,0.35);
#798=CIRCLE('',#7102,0.35);
#799=CIRCLE('',#7104,0.32);
#800=CIRCLE('',#7106,0.22);
#801=CIRCLE('',#7108,0.1954);
#802=CIRCLE('',#7112,0.6);
#803=CIRCLE('',#7113,0.6);
#804=CIRCLE('',#7116,0.275);
#805=CIRCLE('',#7117,0.275);
#806=CIRCLE('',#7119,0.275);
#807=CIRCLE('',#7120,0.275);
#808=CIRCLE('',#7137,0.24505);
#809=CIRCLE('',#7139,0.375);
#810=CIRCLE('',#7141,0.425);
#811=CIRCLE('',#7143,0.425);
#812=CIRCLE('',#7145,0.395);
#813=CIRCLE('',#7147,0.27);
#814=CIRCLE('',#7149,0.24505);
#815=CIRCLE('',#7153,0.21);
#816=CIRCLE('',#7154,0.21);
#817=CIRCLE('',#7156,0.21);
#818=CIRCLE('',#7157,0.21);
#819=CIRCLE('',#7160,0.21);
#820=CIRCLE('',#7161,0.21);
#821=CIRCLE('',#7163,0.21);
#822=CIRCLE('',#7164,0.21);
#823=CIRCLE('',#7167,0.4);
#824=CIRCLE('',#7168,0.4);
#825=CIRCLE('',#7170,0.605);
#826=CIRCLE('',#7171,0.605);
#827=CIRCLE('',#7187,0.22);
#828=CIRCLE('',#7189,0.24505);
#829=CIRCLE('',#7191,0.24505);
#830=CIRCLE('',#7193,0.175);
#831=CIRCLE('',#7197,0.15);
#832=CIRCLE('',#7198,0.15);
#833=CIRCLE('',#7201,0.4);
#834=CIRCLE('',#7204,1.8);
#835=CIRCLE('',#7205,1.8);
#836=CIRCLE('',#7210,1.6);
#837=CIRCLE('',#7211,1.6);
#838=CIRCLE('',#7222,0.15);
#839=CIRCLE('',#7223,0.15);
#840=CIRCLE('',#7228,0.505);
#841=CIRCLE('',#7229,0.505);
#842=CIRCLE('',#7231,0.7);
#843=CIRCLE('',#7232,0.7);
#844=CIRCLE('',#7237,0.505);
#845=CIRCLE('',#7238,0.505);
#846=CIRCLE('',#7240,0.7);
#847=CIRCLE('',#7241,0.7);
#848=CIRCLE('',#7246,0.505);
#849=CIRCLE('',#7247,0.505);
#850=CIRCLE('',#7249,0.7);
#851=CIRCLE('',#7250,0.7);
#852=CIRCLE('',#7315,1.);
#853=CIRCLE('',#7316,1.);
#854=CIRCLE('',#7324,0.976185);
#855=CIRCLE('',#7325,0.976185);
#856=CIRCLE('',#7326,0.247676);
#857=CIRCLE('',#7327,0.976185);
#858=CIRCLE('',#7328,0.976185);
#859=CIRCLE('',#7330,0.976185);
#860=CIRCLE('',#7332,0.5);
#861=CIRCLE('',#7333,0.5);
#862=CIRCLE('',#7335,0.56);
#863=CIRCLE('',#7338,0.976185);
#864=CIRCLE('',#7340,0.56);
#865=CIRCLE('',#7344,1.023815);
#866=CIRCLE('',#7345,1.023815);
#867=CIRCLE('',#7346,0.247676);
#868=CIRCLE('',#7347,1.023815);
#869=CIRCLE('',#7348,1.023815);
#870=CIRCLE('',#7350,1.023815);
#871=CIRCLE('',#7352,1.44);
#872=CIRCLE('',#7353,1.023815);
#873=CIRCLE('',#7355,1.5);
#874=CIRCLE('',#7357,1.5);
#875=CIRCLE('',#7359,1.44);
#876=CIRCLE('',#7364,0.23815);
#877=CIRCLE('',#7366,0.23815);
#878=CIRCLE('',#7368,0.23815);
#879=CIRCLE('',#7370,0.23815);
#880=CIRCLE('',#7372,0.23815);
#881=CIRCLE('',#7374,0.23815);
#882=CIRCLE('',#7376,0.23815);
#883=CIRCLE('',#7378,0.23815);
#884=CIRCLE('',#7381,0.243053047864041);
#885=CIRCLE('',#7382,0.243053047864041);
#886=CIRCLE('',#7384,1.019052);
#887=CIRCLE('',#7385,1.019052);
#888=CIRCLE('',#7386,1.019052);
#889=CIRCLE('',#7387,1.019052);
#890=CIRCLE('',#7388,1.019052);
#891=CIRCLE('',#7389,1.019052);
#892=CIRCLE('',#7390,1.019052);
#893=CIRCLE('',#7391,1.019052);
#894=CIRCLE('',#7392,1.019052);
#895=CIRCLE('',#7394,0.980948);
#896=CIRCLE('',#7395,0.243053047864041);
#897=CIRCLE('',#7397,0.243053047864041);
#898=CIRCLE('',#7399,0.980948);
#899=CIRCLE('',#7400,0.243053047864041);
#900=CIRCLE('',#7402,0.243053047864041);
#901=CIRCLE('',#7404,0.980948);
#902=CIRCLE('',#7405,0.243053047864041);
#903=CIRCLE('',#7407,0.243053047864041);
#904=CIRCLE('',#7409,0.980948);
#905=CIRCLE('',#7410,0.243053047864041);
#906=CIRCLE('',#7412,0.243053047864041);
#907=CIRCLE('',#7414,0.980948);
#908=CIRCLE('',#7415,0.243053047864041);
#909=CIRCLE('',#7417,0.243053047864041);
#910=CIRCLE('',#7419,0.980948);
#911=CIRCLE('',#7420,0.243053047864041);
#912=CIRCLE('',#7422,0.243053047864041);
#913=CIRCLE('',#7424,0.980948);
#914=CIRCLE('',#7425,0.980948);
#915=CIRCLE('',#7426,0.980948);
#916=CIRCLE('',#7428,0.243053047864041);
#917=CIRCLE('',#7430,0.243053047864041);
#918=CIRCLE('',#7435,1.013815);
#919=CIRCLE('',#7436,0.991185);
#920=CIRCLE('',#7438,1.013815);
#921=CIRCLE('',#7440,0.991185);
#922=CIRCLE('',#7443,1.013815);
#923=CIRCLE('',#7444,0.991185);
#924=CIRCLE('',#7446,1.013815);
#925=CIRCLE('',#7448,0.991185);
#926=CIRCLE('',#7457,1.5);
#927=CIRCLE('',#7458,1.5);
#928=CIRCLE('',#7460,1.8);
#929=CIRCLE('',#7461,1.8);
#930=CIRCLE('',#7466,1.1);
#931=CIRCLE('',#7467,1.1);
#932=CIRCLE('',#7469,1.8);
#933=CIRCLE('',#7470,1.8);
#934=CIRCLE('',#7475,1.1);
#935=CIRCLE('',#7476,1.1);
#936=CIRCLE('',#7478,1.8);
#937=CIRCLE('',#7479,1.8);
#938=CYLINDRICAL_SURFACE('',#6773,0.21);
#939=CYLINDRICAL_SURFACE('',#6787,0.21);
#940=CYLINDRICAL_SURFACE('',#6790,0.21);
#941=CYLINDRICAL_SURFACE('',#6793,0.25);
#942=CYLINDRICAL_SURFACE('',#6796,0.25);
#943=CYLINDRICAL_SURFACE('',#6799,0.25);
#944=CYLINDRICAL_SURFACE('',#6802,0.25);
#945=CYLINDRICAL_SURFACE('',#6805,0.275);
#946=CYLINDRICAL_SURFACE('',#6808,0.275);
#947=CYLINDRICAL_SURFACE('',#6811,0.275);
#948=CYLINDRICAL_SURFACE('',#6814,0.275);
#949=CYLINDRICAL_SURFACE('',#6817,0.275);
#950=CYLINDRICAL_SURFACE('',#6820,0.275);
#951=CYLINDRICAL_SURFACE('',#6841,0.2117);
#952=CYLINDRICAL_SURFACE('',#6854,0.265);
#953=CYLINDRICAL_SURFACE('',#6858,0.5);
#954=CYLINDRICAL_SURFACE('',#6876,0.33);
#955=CYLINDRICAL_SURFACE('',#6879,0.33);
#956=CYLINDRICAL_SURFACE('',#6882,1.1);
#957=CYLINDRICAL_SURFACE('',#6889,0.5);
#958=CYLINDRICAL_SURFACE('',#6891,0.5);
#959=CYLINDRICAL_SURFACE('',#6901,0.165);
#960=CYLINDRICAL_SURFACE('',#6908,0.8);
#961=CYLINDRICAL_SURFACE('',#6911,0.5);
#962=CYLINDRICAL_SURFACE('',#6915,0.505);
#963=CYLINDRICAL_SURFACE('',#6918,0.7);
#964=CYLINDRICAL_SURFACE('',#6924,0.505);
#965=CYLINDRICAL_SURFACE('',#6927,0.7);
#966=CYLINDRICAL_SURFACE('',#6933,0.225);
#967=CYLINDRICAL_SURFACE('',#6936,0.8);
#968=CYLINDRICAL_SURFACE('',#6942,0.165);
#969=CYLINDRICAL_SURFACE('',#6949,0.8);
#970=CYLINDRICAL_SURFACE('',#6952,0.5);
#971=CYLINDRICAL_SURFACE('',#6956,0.505);
#972=CYLINDRICAL_SURFACE('',#6959,0.7);
#973=CYLINDRICAL_SURFACE('',#6965,0.225);
#974=CYLINDRICAL_SURFACE('',#6968,0.8);
#975=CYLINDRICAL_SURFACE('',#6974,0.33);
#976=CYLINDRICAL_SURFACE('',#6977,0.33);
#977=CYLINDRICAL_SURFACE('',#6980,1.1);
#978=CYLINDRICAL_SURFACE('',#6987,0.5);
#979=CYLINDRICAL_SURFACE('',#6989,0.5);
#980=CYLINDRICAL_SURFACE('',#7013,0.5);
#981=CYLINDRICAL_SURFACE('',#7021,0.2942);
#982=CYLINDRICAL_SURFACE('',#7023,0.165);
#983=CYLINDRICAL_SURFACE('',#7030,0.8);
#984=CYLINDRICAL_SURFACE('',#7033,0.5);
#985=CYLINDRICAL_SURFACE('',#7037,0.505);
#986=CYLINDRICAL_SURFACE('',#7040,0.7);
#987=CYLINDRICAL_SURFACE('',#7046,0.225);
#988=CYLINDRICAL_SURFACE('',#7049,0.8);
#989=CYLINDRICAL_SURFACE('',#7055,0.165);
#990=CYLINDRICAL_SURFACE('',#7062,0.8);
#991=CYLINDRICAL_SURFACE('',#7065,0.5);
#992=CYLINDRICAL_SURFACE('',#7069,0.505);
#993=CYLINDRICAL_SURFACE('',#7072,0.7);
#994=CYLINDRICAL_SURFACE('',#7078,0.225);
#995=CYLINDRICAL_SURFACE('',#7081,0.8);
#996=CYLINDRICAL_SURFACE('',#7101,0.35);
#997=CYLINDRICAL_SURFACE('',#7109,0.1954);
#998=CYLINDRICAL_SURFACE('',#7111,0.6);
#999=CYLINDRICAL_SURFACE('',#7115,0.275);
#1000=CYLINDRICAL_SURFACE('',#7118,0.275);
#1001=CYLINDRICAL_SURFACE('',#7142,0.425);
#1002=CYLINDRICAL_SURFACE('',#7150,0.24505);
#1003=CYLINDRICAL_SURFACE('',#7155,0.21);
#1004=CYLINDRICAL_SURFACE('',#7162,0.21);
#1005=CYLINDRICAL_SURFACE('',#7166,0.4);
#1006=CYLINDRICAL_SURFACE('',#7169,0.605);
#1007=CYLINDRICAL_SURFACE('',#7190,0.24505);
#1008=CYLINDRICAL_SURFACE('',#7196,0.15);
#1009=CYLINDRICAL_SURFACE('',#7200,0.4);
#1010=CYLINDRICAL_SURFACE('',#7203,1.8);
#1011=CYLINDRICAL_SURFACE('',#7209,1.6);
#1012=CYLINDRICAL_SURFACE('',#7221,0.15);
#1013=CYLINDRICAL_SURFACE('',#7227,0.505);
#1014=CYLINDRICAL_SURFACE('',#7230,0.7);
#1015=CYLINDRICAL_SURFACE('',#7236,0.505);
#1016=CYLINDRICAL_SURFACE('',#7239,0.7);
#1017=CYLINDRICAL_SURFACE('',#7245,0.505);
#1018=CYLINDRICAL_SURFACE('',#7248,0.7);
#1019=CYLINDRICAL_SURFACE('',#7314,1.);
#1020=CYLINDRICAL_SURFACE('',#7329,0.976185);
#1021=CYLINDRICAL_SURFACE('',#7331,0.5);
#1022=CYLINDRICAL_SURFACE('',#7337,0.976185);
#1023=CYLINDRICAL_SURFACE('',#7349,1.023815);
#1024=CYLINDRICAL_SURFACE('',#7356,1.5);
#1025=CYLINDRICAL_SURFACE('',#7361,1.023815);
#1026=CYLINDRICAL_SURFACE('',#7383,1.019052);
#1027=CYLINDRICAL_SURFACE('',#7423,0.980948);
#1028=CYLINDRICAL_SURFACE('',#7437,1.013815);
#1029=CYLINDRICAL_SURFACE('',#7441,0.991185);
#1030=CYLINDRICAL_SURFACE('',#7445,1.013815);
#1031=CYLINDRICAL_SURFACE('',#7449,0.991185);
#1032=CYLINDRICAL_SURFACE('',#7456,1.5);
#1033=CYLINDRICAL_SURFACE('',#7459,1.8);
#1034=CYLINDRICAL_SURFACE('',#7465,1.1);
#1035=CYLINDRICAL_SURFACE('',#7468,1.8);
#1036=CYLINDRICAL_SURFACE('',#7474,1.1);
#1037=CYLINDRICAL_SURFACE('',#7477,1.8);
#1038=FACE_OUTER_BOUND('',#1406,.T.);
#1039=FACE_OUTER_BOUND('',#1407,.T.);
#1040=FACE_OUTER_BOUND('',#1408,.T.);
#1041=FACE_OUTER_BOUND('',#1409,.T.);
#1042=FACE_OUTER_BOUND('',#1410,.T.);
#1043=FACE_OUTER_BOUND('',#1411,.T.);
#1044=FACE_OUTER_BOUND('',#1412,.T.);
#1045=FACE_OUTER_BOUND('',#1413,.T.);
#1046=FACE_OUTER_BOUND('',#1414,.T.);
#1047=FACE_OUTER_BOUND('',#1415,.T.);
#1048=FACE_OUTER_BOUND('',#1416,.T.);
#1049=FACE_OUTER_BOUND('',#1417,.T.);
#1050=FACE_OUTER_BOUND('',#1418,.T.);
#1051=FACE_OUTER_BOUND('',#1419,.T.);
#1052=FACE_OUTER_BOUND('',#1420,.T.);
#1053=FACE_OUTER_BOUND('',#1421,.T.);
#1054=FACE_OUTER_BOUND('',#1422,.T.);
#1055=FACE_OUTER_BOUND('',#1423,.T.);
#1056=FACE_OUTER_BOUND('',#1424,.T.);
#1057=FACE_OUTER_BOUND('',#1425,.T.);
#1058=FACE_OUTER_BOUND('',#1426,.T.);
#1059=FACE_OUTER_BOUND('',#1427,.T.);
#1060=FACE_OUTER_BOUND('',#1428,.T.);
#1061=FACE_OUTER_BOUND('',#1429,.T.);
#1062=FACE_OUTER_BOUND('',#1430,.T.);
#1063=FACE_OUTER_BOUND('',#1431,.T.);
#1064=FACE_OUTER_BOUND('',#1432,.T.);
#1065=FACE_OUTER_BOUND('',#1433,.T.);
#1066=FACE_OUTER_BOUND('',#1434,.T.);
#1067=FACE_OUTER_BOUND('',#1435,.T.);
#1068=FACE_OUTER_BOUND('',#1436,.T.);
#1069=FACE_OUTER_BOUND('',#1437,.T.);
#1070=FACE_OUTER_BOUND('',#1438,.T.);
#1071=FACE_OUTER_BOUND('',#1439,.T.);
#1072=FACE_OUTER_BOUND('',#1440,.T.);
#1073=FACE_OUTER_BOUND('',#1441,.T.);
#1074=FACE_OUTER_BOUND('',#1442,.T.);
#1075=FACE_OUTER_BOUND('',#1443,.T.);
#1076=FACE_OUTER_BOUND('',#1444,.T.);
#1077=FACE_OUTER_BOUND('',#1445,.T.);
#1078=FACE_OUTER_BOUND('',#1446,.T.);
#1079=FACE_OUTER_BOUND('',#1447,.T.);
#1080=FACE_OUTER_BOUND('',#1448,.T.);
#1081=FACE_OUTER_BOUND('',#1449,.T.);
#1082=FACE_OUTER_BOUND('',#1450,.T.);
#1083=FACE_OUTER_BOUND('',#1451,.T.);
#1084=FACE_OUTER_BOUND('',#1453,.T.);
#1085=FACE_OUTER_BOUND('',#1455,.T.);
#1086=FACE_OUTER_BOUND('',#1456,.T.);
#1087=FACE_OUTER_BOUND('',#1457,.T.);
#1088=FACE_OUTER_BOUND('',#1458,.T.);
#1089=FACE_OUTER_BOUND('',#1459,.T.);
#1090=FACE_OUTER_BOUND('',#1460,.T.);
#1091=FACE_OUTER_BOUND('',#1461,.T.);
#1092=FACE_OUTER_BOUND('',#1462,.T.);
#1093=FACE_OUTER_BOUND('',#1463,.T.);
#1094=FACE_OUTER_BOUND('',#1464,.T.);
#1095=FACE_OUTER_BOUND('',#1465,.T.);
#1096=FACE_OUTER_BOUND('',#1466,.T.);
#1097=FACE_OUTER_BOUND('',#1467,.T.);
#1098=FACE_OUTER_BOUND('',#1468,.T.);
#1099=FACE_OUTER_BOUND('',#1469,.T.);
#1100=FACE_OUTER_BOUND('',#1470,.T.);
#1101=FACE_OUTER_BOUND('',#1471,.T.);
#1102=FACE_OUTER_BOUND('',#1484,.T.);
#1103=FACE_OUTER_BOUND('',#1497,.T.);
#1104=FACE_OUTER_BOUND('',#1498,.T.);
#1105=FACE_OUTER_BOUND('',#1499,.T.);
#1106=FACE_OUTER_BOUND('',#1501,.T.);
#1107=FACE_OUTER_BOUND('',#1502,.T.);
#1108=FACE_OUTER_BOUND('',#1503,.T.);
#1109=FACE_OUTER_BOUND('',#1504,.T.);
#1110=FACE_OUTER_BOUND('',#1505,.T.);
#1111=FACE_OUTER_BOUND('',#1506,.T.);
#1112=FACE_OUTER_BOUND('',#1507,.T.);
#1113=FACE_OUTER_BOUND('',#1508,.T.);
#1114=FACE_OUTER_BOUND('',#1509,.T.);
#1115=FACE_OUTER_BOUND('',#1510,.T.);
#1116=FACE_OUTER_BOUND('',#1511,.T.);
#1117=FACE_OUTER_BOUND('',#1512,.T.);
#1118=FACE_OUTER_BOUND('',#1513,.T.);
#1119=FACE_OUTER_BOUND('',#1514,.T.);
#1120=FACE_OUTER_BOUND('',#1516,.T.);
#1121=FACE_OUTER_BOUND('',#1517,.T.);
#1122=FACE_OUTER_BOUND('',#1519,.T.);
#1123=FACE_OUTER_BOUND('',#1520,.T.);
#1124=FACE_OUTER_BOUND('',#1521,.T.);
#1125=FACE_OUTER_BOUND('',#1522,.T.);
#1126=FACE_OUTER_BOUND('',#1523,.T.);
#1127=FACE_OUTER_BOUND('',#1524,.T.);
#1128=FACE_OUTER_BOUND('',#1525,.T.);
#1129=FACE_OUTER_BOUND('',#1526,.T.);
#1130=FACE_OUTER_BOUND('',#1527,.T.);
#1131=FACE_OUTER_BOUND('',#1528,.T.);
#1132=FACE_OUTER_BOUND('',#1529,.T.);
#1133=FACE_OUTER_BOUND('',#1530,.T.);
#1134=FACE_OUTER_BOUND('',#1531,.T.);
#1135=FACE_OUTER_BOUND('',#1532,.T.);
#1136=FACE_OUTER_BOUND('',#1533,.T.);
#1137=FACE_OUTER_BOUND('',#1534,.T.);
#1138=FACE_OUTER_BOUND('',#1537,.T.);
#1139=FACE_OUTER_BOUND('',#1538,.T.);
#1140=FACE_OUTER_BOUND('',#1539,.T.);
#1141=FACE_OUTER_BOUND('',#1540,.T.);
#1142=FACE_OUTER_BOUND('',#1543,.T.);
#1143=FACE_OUTER_BOUND('',#1544,.T.);
#1144=FACE_OUTER_BOUND('',#1545,.T.);
#1145=FACE_OUTER_BOUND('',#1548,.T.);
#1146=FACE_OUTER_BOUND('',#1549,.T.);
#1147=FACE_OUTER_BOUND('',#1550,.T.);
#1148=FACE_OUTER_BOUND('',#1553,.T.);
#1149=FACE_OUTER_BOUND('',#1554,.T.);
#1150=FACE_OUTER_BOUND('',#1555,.T.);
#1151=FACE_OUTER_BOUND('',#1557,.T.);
#1152=FACE_OUTER_BOUND('',#1558,.T.);
#1153=FACE_OUTER_BOUND('',#1559,.T.);
#1154=FACE_OUTER_BOUND('',#1560,.T.);
#1155=FACE_OUTER_BOUND('',#1562,.T.);
#1156=FACE_OUTER_BOUND('',#1563,.T.);
#1157=FACE_OUTER_BOUND('',#1564,.T.);
#1158=FACE_OUTER_BOUND('',#1566,.T.);
#1159=FACE_OUTER_BOUND('',#1568,.T.);
#1160=FACE_OUTER_BOUND('',#1569,.T.);
#1161=FACE_OUTER_BOUND('',#1570,.T.);
#1162=FACE_OUTER_BOUND('',#1572,.T.);
#1163=FACE_OUTER_BOUND('',#1574,.T.);
#1164=FACE_OUTER_BOUND('',#1575,.T.);
#1165=FACE_OUTER_BOUND('',#1576,.T.);
#1166=FACE_OUTER_BOUND('',#1578,.T.);
#1167=FACE_OUTER_BOUND('',#1580,.T.);
#1168=FACE_OUTER_BOUND('',#1581,.T.);
#1169=FACE_OUTER_BOUND('',#1582,.T.);
#1170=FACE_OUTER_BOUND('',#1584,.T.);
#1171=FACE_OUTER_BOUND('',#1585,.T.);
#1172=FACE_OUTER_BOUND('',#1586,.T.);
#1173=FACE_OUTER_BOUND('',#1587,.T.);
#1174=FACE_OUTER_BOUND('',#1589,.T.);
#1175=FACE_OUTER_BOUND('',#1590,.T.);
#1176=FACE_OUTER_BOUND('',#1591,.T.);
#1177=FACE_OUTER_BOUND('',#1593,.T.);
#1178=FACE_OUTER_BOUND('',#1595,.T.);
#1179=FACE_OUTER_BOUND('',#1596,.T.);
#1180=FACE_OUTER_BOUND('',#1597,.T.);
#1181=FACE_OUTER_BOUND('',#1599,.T.);
#1182=FACE_OUTER_BOUND('',#1601,.T.);
#1183=FACE_OUTER_BOUND('',#1602,.T.);
#1184=FACE_OUTER_BOUND('',#1603,.T.);
#1185=FACE_OUTER_BOUND('',#1604,.T.);
#1186=FACE_OUTER_BOUND('',#1607,.T.);
#1187=FACE_OUTER_BOUND('',#1608,.T.);
#1188=FACE_OUTER_BOUND('',#1609,.T.);
#1189=FACE_OUTER_BOUND('',#1610,.T.);
#1190=FACE_OUTER_BOUND('',#1613,.T.);
#1191=FACE_OUTER_BOUND('',#1614,.T.);
#1192=FACE_OUTER_BOUND('',#1615,.T.);
#1193=FACE_OUTER_BOUND('',#1618,.T.);
#1194=FACE_OUTER_BOUND('',#1619,.T.);
#1195=FACE_OUTER_BOUND('',#1620,.T.);
#1196=FACE_OUTER_BOUND('',#1623,.T.);
#1197=FACE_OUTER_BOUND('',#1624,.T.);
#1198=FACE_OUTER_BOUND('',#1625,.T.);
#1199=FACE_OUTER_BOUND('',#1626,.T.);
#1200=FACE_OUTER_BOUND('',#1627,.T.);
#1201=FACE_OUTER_BOUND('',#1628,.T.);
#1202=FACE_OUTER_BOUND('',#1629,.T.);
#1203=FACE_OUTER_BOUND('',#1630,.T.);
#1204=FACE_OUTER_BOUND('',#1631,.T.);
#1205=FACE_OUTER_BOUND('',#1632,.T.);
#1206=FACE_OUTER_BOUND('',#1633,.T.);
#1207=FACE_OUTER_BOUND('',#1634,.T.);
#1208=FACE_OUTER_BOUND('',#1635,.T.);
#1209=FACE_OUTER_BOUND('',#1636,.T.);
#1210=FACE_OUTER_BOUND('',#1638,.T.);
#1211=FACE_OUTER_BOUND('',#1639,.T.);
#1212=FACE_OUTER_BOUND('',#1640,.T.);
#1213=FACE_OUTER_BOUND('',#1641,.T.);
#1214=FACE_OUTER_BOUND('',#1642,.T.);
#1215=FACE_OUTER_BOUND('',#1644,.T.);
#1216=FACE_OUTER_BOUND('',#1645,.T.);
#1217=FACE_OUTER_BOUND('',#1646,.T.);
#1218=FACE_OUTER_BOUND('',#1647,.T.);
#1219=FACE_OUTER_BOUND('',#1649,.T.);
#1220=FACE_OUTER_BOUND('',#1650,.T.);
#1221=FACE_OUTER_BOUND('',#1651,.T.);
#1222=FACE_OUTER_BOUND('',#1653,.T.);
#1223=FACE_OUTER_BOUND('',#1655,.T.);
#1224=FACE_OUTER_BOUND('',#1656,.T.);
#1225=FACE_OUTER_BOUND('',#1657,.T.);
#1226=FACE_OUTER_BOUND('',#1659,.T.);
#1227=FACE_OUTER_BOUND('',#1661,.T.);
#1228=FACE_OUTER_BOUND('',#1662,.T.);
#1229=FACE_OUTER_BOUND('',#1663,.T.);
#1230=FACE_OUTER_BOUND('',#1665,.T.);
#1231=FACE_OUTER_BOUND('',#1666,.T.);
#1232=FACE_OUTER_BOUND('',#1667,.T.);
#1233=FACE_OUTER_BOUND('',#1668,.T.);
#1234=FACE_OUTER_BOUND('',#1670,.T.);
#1235=FACE_OUTER_BOUND('',#1671,.T.);
#1236=FACE_OUTER_BOUND('',#1672,.T.);
#1237=FACE_OUTER_BOUND('',#1674,.T.);
#1238=FACE_OUTER_BOUND('',#1676,.T.);
#1239=FACE_OUTER_BOUND('',#1677,.T.);
#1240=FACE_OUTER_BOUND('',#1678,.T.);
#1241=FACE_OUTER_BOUND('',#1680,.T.);
#1242=FACE_OUTER_BOUND('',#1682,.T.);
#1243=FACE_OUTER_BOUND('',#1683,.T.);
#1244=FACE_OUTER_BOUND('',#1684,.T.);
#1245=FACE_OUTER_BOUND('',#1685,.T.);
#1246=FACE_OUTER_BOUND('',#1686,.T.);
#1247=FACE_OUTER_BOUND('',#1687,.T.);
#1248=FACE_OUTER_BOUND('',#1688,.T.);
#1249=FACE_OUTER_BOUND('',#1689,.T.);
#1250=FACE_OUTER_BOUND('',#1690,.T.);
#1251=FACE_OUTER_BOUND('',#1691,.T.);
#1252=FACE_OUTER_BOUND('',#1692,.T.);
#1253=FACE_OUTER_BOUND('',#1693,.T.);
#1254=FACE_OUTER_BOUND('',#1694,.T.);
#1255=FACE_OUTER_BOUND('',#1695,.T.);
#1256=FACE_OUTER_BOUND('',#1697,.T.);
#1257=FACE_OUTER_BOUND('',#1698,.T.);
#1258=FACE_OUTER_BOUND('',#1699,.T.);
#1259=FACE_OUTER_BOUND('',#1700,.T.);
#1260=FACE_OUTER_BOUND('',#1701,.T.);
#1261=FACE_OUTER_BOUND('',#1702,.T.);
#1262=FACE_OUTER_BOUND('',#1703,.T.);
#1263=FACE_OUTER_BOUND('',#1704,.T.);
#1264=FACE_OUTER_BOUND('',#1705,.T.);
#1265=FACE_OUTER_BOUND('',#1706,.T.);
#1266=FACE_OUTER_BOUND('',#1707,.T.);
#1267=FACE_OUTER_BOUND('',#1711,.T.);
#1268=FACE_OUTER_BOUND('',#1714,.T.);
#1269=FACE_OUTER_BOUND('',#1715,.T.);
#1270=FACE_OUTER_BOUND('',#1716,.T.);
#1271=FACE_OUTER_BOUND('',#1717,.T.);
#1272=FACE_OUTER_BOUND('',#1718,.T.);
#1273=FACE_OUTER_BOUND('',#1719,.T.);
#1274=FACE_OUTER_BOUND('',#1720,.T.);
#1275=FACE_OUTER_BOUND('',#1721,.T.);
#1276=FACE_OUTER_BOUND('',#1722,.T.);
#1277=FACE_OUTER_BOUND('',#1723,.T.);
#1278=FACE_OUTER_BOUND('',#1724,.T.);
#1279=FACE_OUTER_BOUND('',#1725,.T.);
#1280=FACE_OUTER_BOUND('',#1726,.T.);
#1281=FACE_OUTER_BOUND('',#1727,.T.);
#1282=FACE_OUTER_BOUND('',#1729,.T.);
#1283=FACE_OUTER_BOUND('',#1730,.T.);
#1284=FACE_OUTER_BOUND('',#1731,.T.);
#1285=FACE_OUTER_BOUND('',#1732,.T.);
#1286=FACE_OUTER_BOUND('',#1733,.T.);
#1287=FACE_OUTER_BOUND('',#1734,.T.);
#1288=FACE_OUTER_BOUND('',#1735,.T.);
#1289=FACE_OUTER_BOUND('',#1736,.T.);
#1290=FACE_OUTER_BOUND('',#1737,.T.);
#1291=FACE_OUTER_BOUND('',#1739,.T.);
#1292=FACE_OUTER_BOUND('',#1741,.T.);
#1293=FACE_OUTER_BOUND('',#1744,.T.);
#1294=FACE_OUTER_BOUND('',#1745,.T.);
#1295=FACE_OUTER_BOUND('',#1746,.T.);
#1296=FACE_OUTER_BOUND('',#1747,.T.);
#1297=FACE_OUTER_BOUND('',#1750,.T.);
#1298=FACE_OUTER_BOUND('',#1753,.T.);
#1299=FACE_OUTER_BOUND('',#1754,.T.);
#1300=FACE_OUTER_BOUND('',#1755,.T.);
#1301=FACE_OUTER_BOUND('',#1756,.T.);
#1302=FACE_OUTER_BOUND('',#1757,.T.);
#1303=FACE_OUTER_BOUND('',#1758,.T.);
#1304=FACE_OUTER_BOUND('',#1759,.T.);
#1305=FACE_OUTER_BOUND('',#1760,.T.);
#1306=FACE_OUTER_BOUND('',#1762,.T.);
#1307=FACE_OUTER_BOUND('',#1763,.T.);
#1308=FACE_OUTER_BOUND('',#1764,.T.);
#1309=FACE_OUTER_BOUND('',#1765,.T.);
#1310=FACE_OUTER_BOUND('',#1766,.T.);
#1311=FACE_OUTER_BOUND('',#1767,.T.);
#1312=FACE_OUTER_BOUND('',#1768,.T.);
#1313=FACE_OUTER_BOUND('',#1769,.T.);
#1314=FACE_OUTER_BOUND('',#1771,.T.);
#1315=FACE_OUTER_BOUND('',#1773,.T.);
#1316=FACE_OUTER_BOUND('',#1774,.T.);
#1317=FACE_OUTER_BOUND('',#1775,.T.);
#1318=FACE_OUTER_BOUND('',#1776,.T.);
#1319=FACE_OUTER_BOUND('',#1777,.T.);
#1320=FACE_OUTER_BOUND('',#1778,.T.);
#1321=FACE_OUTER_BOUND('',#1779,.T.);
#1322=FACE_OUTER_BOUND('',#1780,.T.);
#1323=FACE_OUTER_BOUND('',#1781,.T.);
#1324=FACE_OUTER_BOUND('',#1782,.T.);
#1325=FACE_OUTER_BOUND('',#1783,.T.);
#1326=FACE_OUTER_BOUND('',#1784,.T.);
#1327=FACE_OUTER_BOUND('',#1785,.T.);
#1328=FACE_OUTER_BOUND('',#1786,.T.);
#1329=FACE_OUTER_BOUND('',#1787,.T.);
#1330=FACE_OUTER_BOUND('',#1788,.T.);
#1331=FACE_OUTER_BOUND('',#1790,.T.);
#1332=FACE_OUTER_BOUND('',#1792,.T.);
#1333=FACE_OUTER_BOUND('',#1793,.T.);
#1334=FACE_OUTER_BOUND('',#1794,.T.);
#1335=FACE_OUTER_BOUND('',#1796,.T.);
#1336=FACE_OUTER_BOUND('',#1798,.T.);
#1337=FACE_OUTER_BOUND('',#1799,.T.);
#1338=FACE_OUTER_BOUND('',#1800,.T.);
#1339=FACE_OUTER_BOUND('',#1802,.T.);
#1340=FACE_OUTER_BOUND('',#1804,.T.);
#1341=FACE_OUTER_BOUND('',#1805,.T.);
#1342=FACE_OUTER_BOUND('',#1806,.T.);
#1343=FACE_OUTER_BOUND('',#1807,.T.);
#1344=FACE_OUTER_BOUND('',#1808,.T.);
#1345=FACE_OUTER_BOUND('',#1809,.T.);
#1346=FACE_OUTER_BOUND('',#1810,.T.);
#1347=FACE_OUTER_BOUND('',#1811,.T.);
#1348=FACE_OUTER_BOUND('',#1813,.T.);
#1349=FACE_OUTER_BOUND('',#1814,.T.);
#1350=FACE_OUTER_BOUND('',#1816,.T.);
#1351=FACE_OUTER_BOUND('',#1817,.T.);
#1352=FACE_OUTER_BOUND('',#1818,.T.);
#1353=FACE_OUTER_BOUND('',#1819,.T.);
#1354=FACE_OUTER_BOUND('',#1821,.T.);
#1355=FACE_OUTER_BOUND('',#1822,.T.);
#1356=FACE_OUTER_BOUND('',#1823,.T.);
#1357=FACE_OUTER_BOUND('',#1824,.T.);
#1358=FACE_OUTER_BOUND('',#1826,.T.);
#1359=FACE_OUTER_BOUND('',#1827,.T.);
#1360=FACE_OUTER_BOUND('',#1828,.T.);
#1361=FACE_OUTER_BOUND('',#1829,.T.);
#1362=FACE_OUTER_BOUND('',#1830,.T.);
#1363=FACE_OUTER_BOUND('',#1831,.T.);
#1364=FACE_OUTER_BOUND('',#1832,.T.);
#1365=FACE_OUTER_BOUND('',#1833,.T.);
#1366=FACE_OUTER_BOUND('',#1834,.T.);
#1367=FACE_OUTER_BOUND('',#1835,.T.);
#1368=FACE_OUTER_BOUND('',#1836,.T.);
#1369=FACE_OUTER_BOUND('',#1837,.T.);
#1370=FACE_OUTER_BOUND('',#1838,.T.);
#1371=FACE_OUTER_BOUND('',#1839,.T.);
#1372=FACE_OUTER_BOUND('',#1840,.T.);
#1373=FACE_OUTER_BOUND('',#1841,.T.);
#1374=FACE_OUTER_BOUND('',#1842,.T.);
#1375=FACE_OUTER_BOUND('',#1843,.T.);
#1376=FACE_OUTER_BOUND('',#1844,.T.);
#1377=FACE_OUTER_BOUND('',#1845,.T.);
#1378=FACE_OUTER_BOUND('',#1846,.T.);
#1379=FACE_OUTER_BOUND('',#1847,.T.);
#1380=FACE_OUTER_BOUND('',#1848,.T.);
#1381=FACE_OUTER_BOUND('',#1849,.T.);
#1382=FACE_OUTER_BOUND('',#1850,.T.);
#1383=FACE_OUTER_BOUND('',#1851,.T.);
#1384=FACE_OUTER_BOUND('',#1852,.T.);
#1385=FACE_OUTER_BOUND('',#1854,.T.);
#1386=FACE_OUTER_BOUND('',#1855,.T.);
#1387=FACE_OUTER_BOUND('',#1857,.T.);
#1388=FACE_OUTER_BOUND('',#1858,.T.);
#1389=FACE_OUTER_BOUND('',#1860,.T.);
#1390=FACE_OUTER_BOUND('',#1861,.T.);
#1391=FACE_OUTER_BOUND('',#1863,.T.);
#1392=FACE_OUTER_BOUND('',#1864,.T.);
#1393=FACE_OUTER_BOUND('',#1866,.T.);
#1394=FACE_OUTER_BOUND('',#1867,.T.);
#1395=FACE_OUTER_BOUND('',#1868,.T.);
#1396=FACE_OUTER_BOUND('',#1869,.T.);
#1397=FACE_OUTER_BOUND('',#1871,.T.);
#1398=FACE_OUTER_BOUND('',#1873,.T.);
#1399=FACE_OUTER_BOUND('',#1874,.T.);
#1400=FACE_OUTER_BOUND('',#1875,.T.);
#1401=FACE_OUTER_BOUND('',#1877,.T.);
#1402=FACE_OUTER_BOUND('',#1879,.T.);
#1403=FACE_OUTER_BOUND('',#1880,.T.);
#1404=FACE_OUTER_BOUND('',#1881,.T.);
#1405=FACE_OUTER_BOUND('',#1883,.T.);
#1406=EDGE_LOOP('',(#4088,#4089,#4090,#4091));
#1407=EDGE_LOOP('',(#4092,#4093,#4094,#4095));
#1408=EDGE_LOOP('',(#4096,#4097,#4098,#4099));
#1409=EDGE_LOOP('',(#4100,#4101,#4102,#4103));
#1410=EDGE_LOOP('',(#4104,#4105,#4106,#4107));
#1411=EDGE_LOOP('',(#4108,#4109,#4110,#4111));
#1412=EDGE_LOOP('',(#4112,#4113,#4114,#4115));
#1413=EDGE_LOOP('',(#4116,#4117,#4118,#4119));
#1414=EDGE_LOOP('',(#4120,#4121,#4122,#4123));
#1415=EDGE_LOOP('',(#4124,#4125,#4126,#4127));
#1416=EDGE_LOOP('',(#4128,#4129,#4130,#4131));
#1417=EDGE_LOOP('',(#4132,#4133,#4134,#4135));
#1418=EDGE_LOOP('',(#4136,#4137,#4138,#4139));
#1419=EDGE_LOOP('',(#4140,#4141,#4142,#4143));
#1420=EDGE_LOOP('',(#4144,#4145,#4146,#4147));
#1421=EDGE_LOOP('',(#4148,#4149,#4150,#4151));
#1422=EDGE_LOOP('',(#4152,#4153,#4154,#4155));
#1423=EDGE_LOOP('',(#4156,#4157,#4158,#4159));
#1424=EDGE_LOOP('',(#4160,#4161,#4162,#4163));
#1425=EDGE_LOOP('',(#4164,#4165,#4166,#4167));
#1426=EDGE_LOOP('',(#4168,#4169,#4170,#4171));
#1427=EDGE_LOOP('',(#4172,#4173,#4174,#4175));
#1428=EDGE_LOOP('',(#4176,#4177,#4178,#4179));
#1429=EDGE_LOOP('',(#4180,#4181,#4182,#4183));
#1430=EDGE_LOOP('',(#4184,#4185,#4186,#4187));
#1431=EDGE_LOOP('',(#4188,#4189,#4190,#4191));
#1432=EDGE_LOOP('',(#4192,#4193,#4194,#4195));
#1433=EDGE_LOOP('',(#4196,#4197,#4198,#4199));
#1434=EDGE_LOOP('',(#4200,#4201,#4202,#4203));
#1435=EDGE_LOOP('',(#4204,#4205,#4206,#4207));
#1436=EDGE_LOOP('',(#4208,#4209,#4210,#4211));
#1437=EDGE_LOOP('',(#4212,#4213,#4214,#4215));
#1438=EDGE_LOOP('',(#4216,#4217,#4218,#4219));
#1439=EDGE_LOOP('',(#4220,#4221,#4222,#4223));
#1440=EDGE_LOOP('',(#4224,#4225,#4226,#4227));
#1441=EDGE_LOOP('',(#4228,#4229,#4230,#4231));
#1442=EDGE_LOOP('',(#4232,#4233,#4234,#4235));
#1443=EDGE_LOOP('',(#4236,#4237,#4238,#4239));
#1444=EDGE_LOOP('',(#4240,#4241,#4242,#4243));
#1445=EDGE_LOOP('',(#4244,#4245,#4246,#4247));
#1446=EDGE_LOOP('',(#4248,#4249,#4250,#4251));
#1447=EDGE_LOOP('',(#4252,#4253,#4254,#4255));
#1448=EDGE_LOOP('',(#4256,#4257,#4258,#4259));
#1449=EDGE_LOOP('',(#4260,#4261,#4262,#4263));
#1450=EDGE_LOOP('',(#4264,#4265,#4266,#4267));
#1451=EDGE_LOOP('',(#4268,#4269,#4270,#4271,#4272,#4273,#4274,#4275,#4276,
#4277,#4278,#4279,#4280,#4281,#4282,#4283,#4284,#4285,#4286,#4287,#4288,
#4289,#4290,#4291,#4292,#4293,#4294,#4295,#4296,#4297,#4298,#4299,#4300,
#4301,#4302,#4303,#4304,#4305,#4306,#4307,#4308,#4309,#4310,#4311));
#1452=EDGE_LOOP('',(#4312));
#1453=EDGE_LOOP('',(#4313,#4314,#4315,#4316,#4317,#4318,#4319,#4320,#4321,
#4322,#4323,#4324,#4325,#4326,#4327,#4328,#4329,#4330,#4331,#4332,#4333,
#4334,#4335,#4336,#4337,#4338,#4339,#4340,#4341,#4342,#4343,#4344,#4345,
#4346,#4347,#4348,#4349,#4350,#4351,#4352,#4353,#4354,#4355,#4356));
#1454=EDGE_LOOP('',(#4357));
#1455=EDGE_LOOP('',(#4358,#4359,#4360,#4361));
#1456=EDGE_LOOP('',(#4362,#4363,#4364,#4365));
#1457=EDGE_LOOP('',(#4366,#4367,#4368,#4369));
#1458=EDGE_LOOP('',(#4370,#4371,#4372,#4373));
#1459=EDGE_LOOP('',(#4374,#4375,#4376,#4377));
#1460=EDGE_LOOP('',(#4378,#4379,#4380,#4381));
#1461=EDGE_LOOP('',(#4382,#4383,#4384,#4385));
#1462=EDGE_LOOP('',(#4386,#4387,#4388,#4389));
#1463=EDGE_LOOP('',(#4390,#4391,#4392,#4393));
#1464=EDGE_LOOP('',(#4394,#4395,#4396,#4397));
#1465=EDGE_LOOP('',(#4398,#4399,#4400,#4401));
#1466=EDGE_LOOP('',(#4402,#4403,#4404,#4405));
#1467=EDGE_LOOP('',(#4406,#4407,#4408,#4409));
#1468=EDGE_LOOP('',(#4410,#4411,#4412,#4413));
#1469=EDGE_LOOP('',(#4414,#4415,#4416,#4417));
#1470=EDGE_LOOP('',(#4418,#4419,#4420,#4421));
#1471=EDGE_LOOP('',(#4422,#4423,#4424,#4425));
#1472=EDGE_LOOP('',(#4426));
#1473=EDGE_LOOP('',(#4427));
#1474=EDGE_LOOP('',(#4428));
#1475=EDGE_LOOP('',(#4429));
#1476=EDGE_LOOP('',(#4430));
#1477=EDGE_LOOP('',(#4431));
#1478=EDGE_LOOP('',(#4432));
#1479=EDGE_LOOP('',(#4433));
#1480=EDGE_LOOP('',(#4434));
#1481=EDGE_LOOP('',(#4435));
#1482=EDGE_LOOP('',(#4436));
#1483=EDGE_LOOP('',(#4437));
#1484=EDGE_LOOP('',(#4438,#4439,#4440,#4441));
#1485=EDGE_LOOP('',(#4442));
#1486=EDGE_LOOP('',(#4443));
#1487=EDGE_LOOP('',(#4444));
#1488=EDGE_LOOP('',(#4445));
#1489=EDGE_LOOP('',(#4446));
#1490=EDGE_LOOP('',(#4447));
#1491=EDGE_LOOP('',(#4448));
#1492=EDGE_LOOP('',(#4449));
#1493=EDGE_LOOP('',(#4450));
#1494=EDGE_LOOP('',(#4451));
#1495=EDGE_LOOP('',(#4452));
#1496=EDGE_LOOP('',(#4453));
#1497=EDGE_LOOP('',(#4454,#4455,#4456,#4457));
#1498=EDGE_LOOP('',(#4458,#4459,#4460,#4461));
#1499=EDGE_LOOP('',(#4462,#4463,#4464,#4465));
#1500=EDGE_LOOP('',(#4466));
#1501=EDGE_LOOP('',(#4467,#4468,#4469,#4470,#4471,#4472,#4473,#4474,#4475,
#4476));
#1502=EDGE_LOOP('',(#4477,#4478,#4479,#4480));
#1503=EDGE_LOOP('',(#4481,#4482,#4483,#4484));
#1504=EDGE_LOOP('',(#4485,#4486,#4487,#4488,#4489,#4490,#4491,#4492,#4493,
#4494));
#1505=EDGE_LOOP('',(#4495,#4496,#4497,#4498));
#1506=EDGE_LOOP('',(#4499,#4500,#4501,#4502,#4503,#4504));
#1507=EDGE_LOOP('',(#4505,#4506,#4507,#4508,#4509,#4510,#4511,#4512));
#1508=EDGE_LOOP('',(#4513,#4514,#4515,#4516,#4517));
#1509=EDGE_LOOP('',(#4518,#4519,#4520,#4521));
#1510=EDGE_LOOP('',(#4522,#4523,#4524,#4525,#4526,#4527));
#1511=EDGE_LOOP('',(#4528,#4529,#4530,#4531));
#1512=EDGE_LOOP('',(#4532,#4533,#4534,#4535));
#1513=EDGE_LOOP('',(#4536,#4537,#4538,#4539));
#1514=EDGE_LOOP('',(#4540));
#1515=EDGE_LOOP('',(#4541));
#1516=EDGE_LOOP('',(#4542,#4543,#4544,#4545));
#1517=EDGE_LOOP('',(#4546));
#1518=EDGE_LOOP('',(#4547));
#1519=EDGE_LOOP('',(#4548,#4549,#4550,#4551));
#1520=EDGE_LOOP('',(#4552,#4553,#4554,#4555));
#1521=EDGE_LOOP('',(#4556,#4557,#4558,#4559));
#1522=EDGE_LOOP('',(#4560,#4561,#4562,#4563));
#1523=EDGE_LOOP('',(#4564,#4565,#4566,#4567));
#1524=EDGE_LOOP('',(#4568,#4569,#4570,#4571));
#1525=EDGE_LOOP('',(#4572,#4573,#4574,#4575));
#1526=EDGE_LOOP('',(#4576,#4577,#4578,#4579));
#1527=EDGE_LOOP('',(#4580,#4581,#4582,#4583));
#1528=EDGE_LOOP('',(#4584,#4585,#4586,#4587));
#1529=EDGE_LOOP('',(#4588,#4589,#4590,#4591));
#1530=EDGE_LOOP('',(#4592,#4593,#4594,#4595));
#1531=EDGE_LOOP('',(#4596,#4597,#4598,#4599));
#1532=EDGE_LOOP('',(#4600,#4601,#4602,#4603));
#1533=EDGE_LOOP('',(#4604,#4605,#4606,#4607));
#1534=EDGE_LOOP('',(#4608,#4609,#4610,#4611,#4612,#4613));
#1535=EDGE_LOOP('',(#4614));
#1536=EDGE_LOOP('',(#4615));
#1537=EDGE_LOOP('',(#4616,#4617,#4618,#4619));
#1538=EDGE_LOOP('',(#4620,#4621,#4622,#4623));
#1539=EDGE_LOOP('',(#4624,#4625,#4626,#4627));
#1540=EDGE_LOOP('',(#4628,#4629,#4630,#4631));
#1541=EDGE_LOOP('',(#4632));
#1542=EDGE_LOOP('',(#4633));
#1543=EDGE_LOOP('',(#4634,#4635,#4636,#4637));
#1544=EDGE_LOOP('',(#4638,#4639,#4640,#4641,#4642,#4643));
#1545=EDGE_LOOP('',(#4644,#4645,#4646,#4647,#4648,#4649));
#1546=EDGE_LOOP('',(#4650));
#1547=EDGE_LOOP('',(#4651));
#1548=EDGE_LOOP('',(#4652,#4653,#4654,#4655,#4656,#4657));
#1549=EDGE_LOOP('',(#4658,#4659,#4660,#4661));
#1550=EDGE_LOOP('',(#4662,#4663,#4664,#4665));
#1551=EDGE_LOOP('',(#4666));
#1552=EDGE_LOOP('',(#4667));
#1553=EDGE_LOOP('',(#4668,#4669,#4670,#4671));
#1554=EDGE_LOOP('',(#4672));
#1555=EDGE_LOOP('',(#4673));
#1556=EDGE_LOOP('',(#4674));
#1557=EDGE_LOOP('',(#4675,#4676,#4677,#4678));
#1558=EDGE_LOOP('',(#4679));
#1559=EDGE_LOOP('',(#4680,#4681,#4682,#4683));
#1560=EDGE_LOOP('',(#4684));
#1561=EDGE_LOOP('',(#4685));
#1562=EDGE_LOOP('',(#4686,#4687,#4688,#4689));
#1563=EDGE_LOOP('',(#4690,#4691,#4692,#4693));
#1564=EDGE_LOOP('',(#4694));
#1565=EDGE_LOOP('',(#4695));
#1566=EDGE_LOOP('',(#4696));
#1567=EDGE_LOOP('',(#4697));
#1568=EDGE_LOOP('',(#4698,#4699,#4700,#4701));
#1569=EDGE_LOOP('',(#4702,#4703,#4704,#4705));
#1570=EDGE_LOOP('',(#4706));
#1571=EDGE_LOOP('',(#4707));
#1572=EDGE_LOOP('',(#4708));
#1573=EDGE_LOOP('',(#4709));
#1574=EDGE_LOOP('',(#4710,#4711,#4712,#4713));
#1575=EDGE_LOOP('',(#4714,#4715,#4716,#4717));
#1576=EDGE_LOOP('',(#4718));
#1577=EDGE_LOOP('',(#4719));
#1578=EDGE_LOOP('',(#4720));
#1579=EDGE_LOOP('',(#4721));
#1580=EDGE_LOOP('',(#4722,#4723,#4724,#4725));
#1581=EDGE_LOOP('',(#4726));
#1582=EDGE_LOOP('',(#4727));
#1583=EDGE_LOOP('',(#4728));
#1584=EDGE_LOOP('',(#4729,#4730,#4731,#4732));
#1585=EDGE_LOOP('',(#4733));
#1586=EDGE_LOOP('',(#4734,#4735,#4736,#4737));
#1587=EDGE_LOOP('',(#4738));
#1588=EDGE_LOOP('',(#4739));
#1589=EDGE_LOOP('',(#4740,#4741,#4742,#4743));
#1590=EDGE_LOOP('',(#4744,#4745,#4746,#4747));
#1591=EDGE_LOOP('',(#4748));
#1592=EDGE_LOOP('',(#4749));
#1593=EDGE_LOOP('',(#4750));
#1594=EDGE_LOOP('',(#4751));
#1595=EDGE_LOOP('',(#4752,#4753,#4754,#4755));
#1596=EDGE_LOOP('',(#4756,#4757,#4758,#4759));
#1597=EDGE_LOOP('',(#4760));
#1598=EDGE_LOOP('',(#4761));
#1599=EDGE_LOOP('',(#4762));
#1600=EDGE_LOOP('',(#4763));
#1601=EDGE_LOOP('',(#4764,#4765,#4766,#4767));
#1602=EDGE_LOOP('',(#4768,#4769,#4770,#4771));
#1603=EDGE_LOOP('',(#4772,#4773,#4774,#4775));
#1604=EDGE_LOOP('',(#4776,#4777,#4778,#4779,#4780,#4781));
#1605=EDGE_LOOP('',(#4782));
#1606=EDGE_LOOP('',(#4783));
#1607=EDGE_LOOP('',(#4784,#4785,#4786,#4787));
#1608=EDGE_LOOP('',(#4788,#4789,#4790,#4791));
#1609=EDGE_LOOP('',(#4792,#4793,#4794,#4795));
#1610=EDGE_LOOP('',(#4796,#4797,#4798,#4799));
#1611=EDGE_LOOP('',(#4800));
#1612=EDGE_LOOP('',(#4801));
#1613=EDGE_LOOP('',(#4802,#4803,#4804,#4805));
#1614=EDGE_LOOP('',(#4806,#4807,#4808,#4809,#4810,#4811));
#1615=EDGE_LOOP('',(#4812,#4813,#4814,#4815,#4816,#4817));
#1616=EDGE_LOOP('',(#4818));
#1617=EDGE_LOOP('',(#4819));
#1618=EDGE_LOOP('',(#4820,#4821,#4822,#4823,#4824,#4825));
#1619=EDGE_LOOP('',(#4826,#4827,#4828,#4829));
#1620=EDGE_LOOP('',(#4830,#4831,#4832,#4833));
#1621=EDGE_LOOP('',(#4834));
#1622=EDGE_LOOP('',(#4835));
#1623=EDGE_LOOP('',(#4836,#4837,#4838,#4839));
#1624=EDGE_LOOP('',(#4840,#4841,#4842,#4843));
#1625=EDGE_LOOP('',(#4844,#4845,#4846,#4847));
#1626=EDGE_LOOP('',(#4848,#4849,#4850,#4851));
#1627=EDGE_LOOP('',(#4852,#4853,#4854,#4855));
#1628=EDGE_LOOP('',(#4856,#4857,#4858,#4859));
#1629=EDGE_LOOP('',(#4860,#4861,#4862,#4863,#4864,#4865));
#1630=EDGE_LOOP('',(#4866,#4867,#4868,#4869,#4870,#4871));
#1631=EDGE_LOOP('',(#4872));
#1632=EDGE_LOOP('',(#4873));
#1633=EDGE_LOOP('',(#4874,#4875,#4876,#4877));
#1634=EDGE_LOOP('',(#4878,#4879,#4880,#4881));
#1635=EDGE_LOOP('',(#4882,#4883,#4884,#4885));
#1636=EDGE_LOOP('',(#4886));
#1637=EDGE_LOOP('',(#4887));
#1638=EDGE_LOOP('',(#4888,#4889,#4890,#4891));
#1639=EDGE_LOOP('',(#4892,#4893,#4894,#4895));
#1640=EDGE_LOOP('',(#4896,#4897,#4898,#4899));
#1641=EDGE_LOOP('',(#4900));
#1642=EDGE_LOOP('',(#4901));
#1643=EDGE_LOOP('',(#4902));
#1644=EDGE_LOOP('',(#4903,#4904,#4905,#4906));
#1645=EDGE_LOOP('',(#4907));
#1646=EDGE_LOOP('',(#4908,#4909,#4910,#4911));
#1647=EDGE_LOOP('',(#4912));
#1648=EDGE_LOOP('',(#4913));
#1649=EDGE_LOOP('',(#4914,#4915,#4916,#4917));
#1650=EDGE_LOOP('',(#4918,#4919,#4920,#4921));
#1651=EDGE_LOOP('',(#4922));
#1652=EDGE_LOOP('',(#4923));
#1653=EDGE_LOOP('',(#4924));
#1654=EDGE_LOOP('',(#4925));
#1655=EDGE_LOOP('',(#4926,#4927,#4928,#4929));
#1656=EDGE_LOOP('',(#4930,#4931,#4932,#4933));
#1657=EDGE_LOOP('',(#4934));
#1658=EDGE_LOOP('',(#4935));
#1659=EDGE_LOOP('',(#4936));
#1660=EDGE_LOOP('',(#4937));
#1661=EDGE_LOOP('',(#4938,#4939,#4940,#4941));
#1662=EDGE_LOOP('',(#4942));
#1663=EDGE_LOOP('',(#4943));
#1664=EDGE_LOOP('',(#4944));
#1665=EDGE_LOOP('',(#4945,#4946,#4947,#4948));
#1666=EDGE_LOOP('',(#4949));
#1667=EDGE_LOOP('',(#4950,#4951,#4952,#4953));
#1668=EDGE_LOOP('',(#4954));
#1669=EDGE_LOOP('',(#4955));
#1670=EDGE_LOOP('',(#4956,#4957,#4958,#4959));
#1671=EDGE_LOOP('',(#4960,#4961,#4962,#4963));
#1672=EDGE_LOOP('',(#4964));
#1673=EDGE_LOOP('',(#4965));
#1674=EDGE_LOOP('',(#4966));
#1675=EDGE_LOOP('',(#4967));
#1676=EDGE_LOOP('',(#4968,#4969,#4970,#4971));
#1677=EDGE_LOOP('',(#4972,#4973,#4974,#4975));
#1678=EDGE_LOOP('',(#4976));
#1679=EDGE_LOOP('',(#4977));
#1680=EDGE_LOOP('',(#4978));
#1681=EDGE_LOOP('',(#4979));
#1682=EDGE_LOOP('',(#4980,#4981,#4982,#4983));
#1683=EDGE_LOOP('',(#4984,#4985,#4986,#4987));
#1684=EDGE_LOOP('',(#4988,#4989,#4990,#4991));
#1685=EDGE_LOOP('',(#4992,#4993,#4994,#4995));
#1686=EDGE_LOOP('',(#4996,#4997,#4998,#4999));
#1687=EDGE_LOOP('',(#5000,#5001,#5002,#5003));
#1688=EDGE_LOOP('',(#5004,#5005,#5006,#5007,#5008,#5009));
#1689=EDGE_LOOP('',(#5010,#5011,#5012,#5013,#5014,#5015));
#1690=EDGE_LOOP('',(#5016));
#1691=EDGE_LOOP('',(#5017));
#1692=EDGE_LOOP('',(#5018,#5019,#5020,#5021));
#1693=EDGE_LOOP('',(#5022,#5023,#5024,#5025));
#1694=EDGE_LOOP('',(#5026,#5027,#5028,#5029));
#1695=EDGE_LOOP('',(#5030));
#1696=EDGE_LOOP('',(#5031));
#1697=EDGE_LOOP('',(#5032,#5033,#5034,#5035));
#1698=EDGE_LOOP('',(#5036,#5037,#5038,#5039));
#1699=EDGE_LOOP('',(#5040,#5041,#5042,#5043));
#1700=EDGE_LOOP('',(#5044));
#1701=EDGE_LOOP('',(#5045,#5046,#5047,#5048));
#1702=EDGE_LOOP('',(#5049,#5050,#5051,#5052));
#1703=EDGE_LOOP('',(#5053,#5054,#5055,#5056));
#1704=EDGE_LOOP('',(#5057,#5058,#5059,#5060));
#1705=EDGE_LOOP('',(#5061,#5062,#5063,#5064));
#1706=EDGE_LOOP('',(#5065,#5066,#5067,#5068));
#1707=EDGE_LOOP('',(#5069,#5070,#5071,#5072));
#1708=EDGE_LOOP('',(#5073));
#1709=EDGE_LOOP('',(#5074));
#1710=EDGE_LOOP('',(#5075));
#1711=EDGE_LOOP('',(#5076,#5077,#5078,#5079));
#1712=EDGE_LOOP('',(#5080));
#1713=EDGE_LOOP('',(#5081));
#1714=EDGE_LOOP('',(#5082,#5083,#5084,#5085));
#1715=EDGE_LOOP('',(#5086,#5087,#5088,#5089));
#1716=EDGE_LOOP('',(#5090,#5091,#5092,#5093));
#1717=EDGE_LOOP('',(#5094,#5095,#5096,#5097));
#1718=EDGE_LOOP('',(#5098,#5099,#5100,#5101));
#1719=EDGE_LOOP('',(#5102,#5103,#5104,#5105));
#1720=EDGE_LOOP('',(#5106,#5107,#5108,#5109,#5110,#5111));
#1721=EDGE_LOOP('',(#5112,#5113,#5114,#5115,#5116,#5117));
#1722=EDGE_LOOP('',(#5118));
#1723=EDGE_LOOP('',(#5119));
#1724=EDGE_LOOP('',(#5120,#5121,#5122,#5123));
#1725=EDGE_LOOP('',(#5124,#5125,#5126,#5127));
#1726=EDGE_LOOP('',(#5128,#5129,#5130,#5131));
#1727=EDGE_LOOP('',(#5132));
#1728=EDGE_LOOP('',(#5133));
#1729=EDGE_LOOP('',(#5134,#5135,#5136,#5137));
#1730=EDGE_LOOP('',(#5138,#5139,#5140,#5141));
#1731=EDGE_LOOP('',(#5142,#5143,#5144));
#1732=EDGE_LOOP('',(#5145,#5146,#5147,#5148,#5149,#5150,#5151,#5152));
#1733=EDGE_LOOP('',(#5153,#5154));
#1734=EDGE_LOOP('',(#5155,#5156,#5157));
#1735=EDGE_LOOP('',(#5158,#5159,#5160,#5161,#5162,#5163,#5164,#5165));
#1736=EDGE_LOOP('',(#5166,#5167));
#1737=EDGE_LOOP('',(#5168,#5169,#5170,#5171));
#1738=EDGE_LOOP('',(#5172,#5173,#5174,#5175));
#1739=EDGE_LOOP('',(#5176,#5177,#5178,#5179));
#1740=EDGE_LOOP('',(#5180,#5181,#5182,#5183));
#1741=EDGE_LOOP('',(#5184,#5185,#5186,#5187));
#1742=EDGE_LOOP('',(#5188));
#1743=EDGE_LOOP('',(#5189));
#1744=EDGE_LOOP('',(#5190,#5191,#5192,#5193));
#1745=EDGE_LOOP('',(#5194,#5195,#5196,#5197));
#1746=EDGE_LOOP('',(#5198,#5199,#5200,#5201));
#1747=EDGE_LOOP('',(#5202,#5203,#5204,#5205));
#1748=EDGE_LOOP('',(#5206));
#1749=EDGE_LOOP('',(#5207));
#1750=EDGE_LOOP('',(#5208,#5209,#5210,#5211));
#1751=EDGE_LOOP('',(#5212));
#1752=EDGE_LOOP('',(#5213));
#1753=EDGE_LOOP('',(#5214,#5215,#5216,#5217));
#1754=EDGE_LOOP('',(#5218,#5219,#5220,#5221));
#1755=EDGE_LOOP('',(#5222,#5223,#5224,#5225));
#1756=EDGE_LOOP('',(#5226,#5227,#5228,#5229));
#1757=EDGE_LOOP('',(#5230,#5231,#5232,#5233));
#1758=EDGE_LOOP('',(#5234,#5235,#5236,#5237));
#1759=EDGE_LOOP('',(#5238,#5239,#5240,#5241,#5242,#5243));
#1760=EDGE_LOOP('',(#5244));
#1761=EDGE_LOOP('',(#5245,#5246,#5247,#5248,#5249,#5250));
#1762=EDGE_LOOP('',(#5251,#5252,#5253,#5254));
#1763=EDGE_LOOP('',(#5255,#5256,#5257,#5258));
#1764=EDGE_LOOP('',(#5259,#5260,#5261,#5262));
#1765=EDGE_LOOP('',(#5263));
#1766=EDGE_LOOP('',(#5264,#5265,#5266,#5267));
#1767=EDGE_LOOP('',(#5268));
#1768=EDGE_LOOP('',(#5269,#5270,#5271,#5272,#5273));
#1769=EDGE_LOOP('',(#5274));
#1770=EDGE_LOOP('',(#5275));
#1771=EDGE_LOOP('',(#5276,#5277,#5278,#5279));
#1772=EDGE_LOOP('',(#5280,#5281));
#1773=EDGE_LOOP('',(#5282));
#1774=EDGE_LOOP('',(#5283));
#1775=EDGE_LOOP('',(#5284,#5285,#5286,#5287));
#1776=EDGE_LOOP('',(#5288));
#1777=EDGE_LOOP('',(#5289));
#1778=EDGE_LOOP('',(#5290,#5291,#5292,#5293));
#1779=EDGE_LOOP('',(#5294,#5295,#5296,#5297));
#1780=EDGE_LOOP('',(#5298,#5299,#5300,#5301));
#1781=EDGE_LOOP('',(#5302,#5303,#5304));
#1782=EDGE_LOOP('',(#5305,#5306,#5307));
#1783=EDGE_LOOP('',(#5308,#5309,#5310,#5311));
#1784=EDGE_LOOP('',(#5312));
#1785=EDGE_LOOP('',(#5313));
#1786=EDGE_LOOP('',(#5314,#5315,#5316,#5317));
#1787=EDGE_LOOP('',(#5318,#5319,#5320,#5321));
#1788=EDGE_LOOP('',(#5322));
#1789=EDGE_LOOP('',(#5323));
#1790=EDGE_LOOP('',(#5324));
#1791=EDGE_LOOP('',(#5325));
#1792=EDGE_LOOP('',(#5326,#5327,#5328,#5329));
#1793=EDGE_LOOP('',(#5330,#5331,#5332,#5333));
#1794=EDGE_LOOP('',(#5334));
#1795=EDGE_LOOP('',(#5335));
#1796=EDGE_LOOP('',(#5336));
#1797=EDGE_LOOP('',(#5337));
#1798=EDGE_LOOP('',(#5338,#5339,#5340,#5341));
#1799=EDGE_LOOP('',(#5342,#5343,#5344,#5345));
#1800=EDGE_LOOP('',(#5346));
#1801=EDGE_LOOP('',(#5347));
#1802=EDGE_LOOP('',(#5348));
#1803=EDGE_LOOP('',(#5349));
#1804=EDGE_LOOP('',(#5350,#5351,#5352,#5353));
#1805=EDGE_LOOP('',(#5354));
#1806=EDGE_LOOP('',(#5355));
#1807=EDGE_LOOP('',(#5356,#5357,#5358,#5359,#5360,#5361));
#1808=EDGE_LOOP('',(#5362,#5363,#5364,#5365,#5366));
#1809=EDGE_LOOP('',(#5367,#5368,#5369,#5370));
#1810=EDGE_LOOP('',(#5371,#5372,#5373,#5374));
#1811=EDGE_LOOP('',(#5375));
#1812=EDGE_LOOP('',(#5376));
#1813=EDGE_LOOP('',(#5377,#5378,#5379,#5380,#5381));
#1814=EDGE_LOOP('',(#5382));
#1815=EDGE_LOOP('',(#5383));
#1816=EDGE_LOOP('',(#5384,#5385,#5386,#5387));
#1817=EDGE_LOOP('',(#5388,#5389,#5390,#5391,#5392,#5393));
#1818=EDGE_LOOP('',(#5394,#5395,#5396,#5397,#5398));
#1819=EDGE_LOOP('',(#5399));
#1820=EDGE_LOOP('',(#5400));
#1821=EDGE_LOOP('',(#5401,#5402,#5403,#5404));
#1822=EDGE_LOOP('',(#5405,#5406,#5407,#5408));
#1823=EDGE_LOOP('',(#5409,#5410,#5411,#5412));
#1824=EDGE_LOOP('',(#5413));
#1825=EDGE_LOOP('',(#5414));
#1826=EDGE_LOOP('',(#5415,#5416,#5417,#5418,#5419));
#1827=EDGE_LOOP('',(#5420,#5421));
#1828=EDGE_LOOP('',(#5422,#5423));
#1829=EDGE_LOOP('',(#5424,#5425));
#1830=EDGE_LOOP('',(#5426,#5427));
#1831=EDGE_LOOP('',(#5428,#5429));
#1832=EDGE_LOOP('',(#5430,#5431));
#1833=EDGE_LOOP('',(#5432,#5433));
#1834=EDGE_LOOP('',(#5434,#5435));
#1835=EDGE_LOOP('',(#5436,#5437,#5438,#5439));
#1836=EDGE_LOOP('',(#5440,#5441,#5442,#5443,#5444,#5445,#5446,#5447,#5448,
#5449,#5450,#5451,#5452,#5453,#5454,#5455,#5456,#5457,#5458,#5459));
#1837=EDGE_LOOP('',(#5460,#5461,#5462,#5463));
#1838=EDGE_LOOP('',(#5464,#5465,#5466,#5467));
#1839=EDGE_LOOP('',(#5468,#5469,#5470,#5471));
#1840=EDGE_LOOP('',(#5472,#5473,#5474,#5475));
#1841=EDGE_LOOP('',(#5476,#5477,#5478,#5479));
#1842=EDGE_LOOP('',(#5480,#5481,#5482,#5483,#5484,#5485));
#1843=EDGE_LOOP('',(#5486,#5487,#5488,#5489));
#1844=EDGE_LOOP('',(#5490,#5491,#5492,#5493));
#1845=EDGE_LOOP('',(#5494,#5495,#5496,#5497));
#1846=EDGE_LOOP('',(#5498,#5499,#5500,#5501));
#1847=EDGE_LOOP('',(#5502,#5503,#5504,#5505));
#1848=EDGE_LOOP('',(#5506,#5507,#5508,#5509));
#1849=EDGE_LOOP('',(#5510,#5511,#5512,#5513,#5514,#5515,#5516,#5517,#5518,
#5519,#5520,#5521,#5522,#5523,#5524,#5525,#5526,#5527,#5528,#5529));
#1850=EDGE_LOOP('',(#5530,#5531,#5532,#5533));
#1851=EDGE_LOOP('',(#5534,#5535,#5536,#5537));
#1852=EDGE_LOOP('',(#5538));
#1853=EDGE_LOOP('',(#5539));
#1854=EDGE_LOOP('',(#5540,#5541,#5542,#5543));
#1855=EDGE_LOOP('',(#5544));
#1856=EDGE_LOOP('',(#5545));
#1857=EDGE_LOOP('',(#5546,#5547,#5548,#5549));
#1858=EDGE_LOOP('',(#5550));
#1859=EDGE_LOOP('',(#5551));
#1860=EDGE_LOOP('',(#5552,#5553,#5554,#5555));
#1861=EDGE_LOOP('',(#5556));
#1862=EDGE_LOOP('',(#5557));
#1863=EDGE_LOOP('',(#5558,#5559,#5560,#5561));
#1864=EDGE_LOOP('',(#5562));
#1865=EDGE_LOOP('',(#5563));
#1866=EDGE_LOOP('',(#5564,#5565,#5566,#5567));
#1867=EDGE_LOOP('',(#5568,#5569,#5570,#5571));
#1868=EDGE_LOOP('',(#5572,#5573,#5574,#5575));
#1869=EDGE_LOOP('',(#5576));
#1870=EDGE_LOOP('',(#5577));
#1871=EDGE_LOOP('',(#5578));
#1872=EDGE_LOOP('',(#5579));
#1873=EDGE_LOOP('',(#5580,#5581,#5582,#5583));
#1874=EDGE_LOOP('',(#5584,#5585,#5586,#5587));
#1875=EDGE_LOOP('',(#5588));
#1876=EDGE_LOOP('',(#5589));
#1877=EDGE_LOOP('',(#5590));
#1878=EDGE_LOOP('',(#5591));
#1879=EDGE_LOOP('',(#5592,#5593,#5594,#5595));
#1880=EDGE_LOOP('',(#5596,#5597,#5598,#5599));
#1881=EDGE_LOOP('',(#5600));
#1882=EDGE_LOOP('',(#5601));
#1883=EDGE_LOOP('',(#5602));
#1884=EDGE_LOOP('',(#5603));
#1885=LINE('',#9481,#2352);
#1886=LINE('',#9483,#2353);
#1887=LINE('',#9485,#2354);
#1888=LINE('',#9486,#2355);
#1889=LINE('',#9489,#2356);
#1890=LINE('',#9491,#2357);
#1891=LINE('',#9492,#2358);
#1892=LINE('',#9495,#2359);
#1893=LINE('',#9497,#2360);
#1894=LINE('',#9498,#2361);
#1895=LINE('',#9501,#2362);
#1896=LINE('',#9503,#2363);
#1897=LINE('',#9504,#2364);
#1898=LINE('',#9507,#2365);
#1899=LINE('',#9509,#2366);
#1900=LINE('',#9510,#2367);
#1901=LINE('',#9513,#2368);
#1902=LINE('',#9515,#2369);
#1903=LINE('',#9516,#2370);
#1904=LINE('',#9519,#2371);
#1905=LINE('',#9521,#2372);
#1906=LINE('',#9522,#2373);
#1907=LINE('',#9525,#2374);
#1908=LINE('',#9527,#2375);
#1909=LINE('',#9528,#2376);
#1910=LINE('',#9531,#2377);
#1911=LINE('',#9533,#2378);
#1912=LINE('',#9534,#2379);
#1913=LINE('',#9538,#2380);
#1914=LINE('',#9540,#2381);
#1915=LINE('',#9542,#2382);
#1916=LINE('',#9543,#2383);
#1917=LINE('',#9546,#2384);
#1918=LINE('',#9548,#2385);
#1919=LINE('',#9549,#2386);
#1920=LINE('',#9552,#2387);
#1921=LINE('',#9554,#2388);
#1922=LINE('',#9555,#2389);
#1923=LINE('',#9558,#2390);
#1924=LINE('',#9560,#2391);
#1925=LINE('',#9561,#2392);
#1926=LINE('',#9564,#2393);
#1927=LINE('',#9566,#2394);
#1928=LINE('',#9567,#2395);
#1929=LINE('',#9570,#2396);
#1930=LINE('',#9572,#2397);
#1931=LINE('',#9573,#2398);
#1932=LINE('',#9576,#2399);
#1933=LINE('',#9578,#2400);
#1934=LINE('',#9579,#2401);
#1935=LINE('',#9582,#2402);
#1936=LINE('',#9584,#2403);
#1937=LINE('',#9585,#2404);
#1938=LINE('',#9588,#2405);
#1939=LINE('',#9590,#2406);
#1940=LINE('',#9591,#2407);
#1941=LINE('',#9595,#2408);
#1942=LINE('',#9597,#2409);
#1943=LINE('',#9599,#2410);
#1944=LINE('',#9600,#2411);
#1945=LINE('',#9603,#2412);
#1946=LINE('',#9605,#2413);
#1947=LINE('',#9606,#2414);
#1948=LINE('',#9609,#2415);
#1949=LINE('',#9611,#2416);
#1950=LINE('',#9612,#2417);
#1951=LINE('',#9615,#2418);
#1952=LINE('',#9617,#2419);
#1953=LINE('',#9618,#2420);
#1954=LINE('',#9621,#2421);
#1955=LINE('',#9623,#2422);
#1956=LINE('',#9624,#2423);
#1957=LINE('',#9627,#2424);
#1958=LINE('',#9629,#2425);
#1959=LINE('',#9630,#2426);
#1960=LINE('',#9633,#2427);
#1961=LINE('',#9635,#2428);
#1962=LINE('',#9636,#2429);
#1963=LINE('',#9639,#2430);
#1964=LINE('',#9641,#2431);
#1965=LINE('',#9642,#2432);
#1966=LINE('',#9645,#2433);
#1967=LINE('',#9647,#2434);
#1968=LINE('',#9648,#2435);
#1969=LINE('',#9652,#2436);
#1970=LINE('',#9654,#2437);
#1971=LINE('',#9656,#2438);
#1972=LINE('',#9657,#2439);
#1973=LINE('',#9660,#2440);
#1974=LINE('',#9662,#2441);
#1975=LINE('',#9663,#2442);
#1976=LINE('',#9666,#2443);
#1977=LINE('',#9668,#2444);
#1978=LINE('',#9669,#2445);
#1979=LINE('',#9672,#2446);
#1980=LINE('',#9674,#2447);
#1981=LINE('',#9675,#2448);
#1982=LINE('',#9678,#2449);
#1983=LINE('',#9680,#2450);
#1984=LINE('',#9681,#2451);
#1985=LINE('',#9684,#2452);
#1986=LINE('',#9686,#2453);
#1987=LINE('',#9687,#2454);
#1988=LINE('',#9690,#2455);
#1989=LINE('',#9692,#2456);
#1990=LINE('',#9693,#2457);
#1991=LINE('',#9696,#2458);
#1992=LINE('',#9698,#2459);
#1993=LINE('',#9699,#2460);
#1994=LINE('',#9702,#2461);
#1995=LINE('',#9704,#2462);
#1996=LINE('',#9705,#2463);
#1997=LINE('',#9710,#2464);
#1998=LINE('',#9714,#2465);
#1999=LINE('',#9716,#2466);
#2000=LINE('',#9717,#2467);
#2001=LINE('',#9720,#2468);
#2002=LINE('',#9722,#2469);
#2003=LINE('',#9723,#2470);
#2004=LINE('',#9725,#2471);
#2005=LINE('',#9726,#2472);
#2006=LINE('',#9729,#2473);
#2007=LINE('',#9731,#2474);
#2008=LINE('',#9732,#2475);
#2009=LINE('',#9734,#2476);
#2010=LINE('',#9735,#2477);
#2011=LINE('',#9738,#2478);
#2012=LINE('',#9740,#2479);
#2013=LINE('',#9741,#2480);
#2014=LINE('',#9743,#2481);
#2015=LINE('',#9744,#2482);
#2016=LINE('',#9746,#2483);
#2017=LINE('',#9747,#2484);
#2018=LINE('',#9755,#2485);
#2019=LINE('',#9761,#2486);
#2020=LINE('',#9767,#2487);
#2021=LINE('',#9773,#2488);
#2022=LINE('',#9779,#2489);
#2023=LINE('',#9785,#2490);
#2024=LINE('',#9791,#2491);
#2025=LINE('',#9797,#2492);
#2026=LINE('',#9803,#2493);
#2027=LINE('',#9809,#2494);
#2028=LINE('',#9815,#2495);
#2029=LINE('',#9821,#2496);
#2030=LINE('',#9826,#2497);
#2031=LINE('',#9828,#2498);
#2032=LINE('',#9830,#2499);
#2033=LINE('',#9831,#2500);
#2034=LINE('',#9834,#2501);
#2035=LINE('',#9836,#2502);
#2036=LINE('',#9837,#2503);
#2037=LINE('',#9840,#2504);
#2038=LINE('',#9842,#2505);
#2039=LINE('',#9843,#2506);
#2040=LINE('',#9845,#2507);
#2041=LINE('',#9846,#2508);
#2042=LINE('',#9853,#2509);
#2043=LINE('',#9855,#2510);
#2044=LINE('',#9857,#2511);
#2045=LINE('',#9858,#2512);
#2046=LINE('',#9861,#2513);
#2047=LINE('',#9863,#2514);
#2048=LINE('',#9864,#2515);
#2049=LINE('',#9867,#2516);
#2050=LINE('',#9869,#2517);
#2051=LINE('',#9870,#2518);
#2052=LINE('',#9875,#2519);
#2053=LINE('',#9877,#2520);
#2054=LINE('',#9879,#2521);
#2055=LINE('',#9881,#2522);
#2056=LINE('',#9883,#2523);
#2057=LINE('',#9885,#2524);
#2058=LINE('',#9886,#2525);
#2059=LINE('',#9889,#2526);
#2060=LINE('',#9890,#2527);
#2061=LINE('',#9893,#2528);
#2062=LINE('',#9894,#2529);
#2063=LINE('',#9897,#2530);
#2064=LINE('',#9899,#2531);
#2065=LINE('',#9901,#2532);
#2066=LINE('',#9903,#2533);
#2067=LINE('',#9904,#2534);
#2068=LINE('',#9906,#2535);
#2069=LINE('',#9909,#2536);
#2070=LINE('',#9912,#2537);
#2071=LINE('',#9916,#2538);
#2072=LINE('',#9923,#2539);
#2073=LINE('',#9925,#2540);
#2074=LINE('',#9927,#2541);
#2075=LINE('',#9934,#2542);
#2076=LINE('',#9938,#2543);
#2077=LINE('',#9945,#2544);
#2078=LINE('',#9952,#2545);
#2079=LINE('',#9954,#2546);
#2080=LINE('',#9956,#2547);
#2081=LINE('',#9957,#2548);
#2082=LINE('',#9960,#2549);
#2083=LINE('',#9962,#2550);
#2084=LINE('',#9963,#2551);
#2085=LINE('',#9966,#2552);
#2086=LINE('',#9968,#2553);
#2087=LINE('',#9969,#2554);
#2088=LINE('',#9971,#2555);
#2089=LINE('',#9972,#2556);
#2090=LINE('',#9979,#2557);
#2091=LINE('',#9981,#2558);
#2092=LINE('',#9983,#2559);
#2093=LINE('',#9984,#2560);
#2094=LINE('',#9987,#2561);
#2095=LINE('',#9989,#2562);
#2096=LINE('',#9990,#2563);
#2097=LINE('',#9993,#2564);
#2098=LINE('',#9995,#2565);
#2099=LINE('',#9996,#2566);
#2100=LINE('',#9998,#2567);
#2101=LINE('',#9999,#2568);
#2102=LINE('',#10007,#2569);
#2103=LINE('',#10013,#2570);
#2104=LINE('',#10020,#2571);
#2105=LINE('',#10023,#2572);
#2106=LINE('',#10026,#2573);
#2107=LINE('',#10028,#2574);
#2108=LINE('',#10030,#2575);
#2109=LINE('',#10032,#2576);
#2110=LINE('',#10033,#2577);
#2111=LINE('',#10040,#2578);
#2112=LINE('',#10041,#2579);
#2113=LINE('',#10045,#2580);
#2114=LINE('',#10049,#2581);
#2115=LINE('',#10053,#2582);
#2116=LINE('',#10055,#2583);
#2117=LINE('',#10057,#2584);
#2118=LINE('',#10058,#2585);
#2119=LINE('',#10061,#2586);
#2120=LINE('',#10063,#2587);
#2121=LINE('',#10064,#2588);
#2122=LINE('',#10066,#2589);
#2123=LINE('',#10067,#2590);
#2124=LINE('',#10070,#2591);
#2125=LINE('',#10071,#2592);
#2126=LINE('',#10073,#2593);
#2127=LINE('',#10074,#2594);
#2128=LINE('',#10082,#2595);
#2129=LINE('',#10092,#2596);
#2130=LINE('',#10098,#2597);
#2131=LINE('',#10105,#2598);
#2132=LINE('',#10111,#2599);
#2133=LINE('',#10120,#2600);
#2134=LINE('',#10126,#2601);
#2135=LINE('',#10135,#2602);
#2136=LINE('',#10141,#2603);
#2137=LINE('',#10150,#2604);
#2138=LINE('',#10160,#2605);
#2139=LINE('',#10166,#2606);
#2140=LINE('',#10173,#2607);
#2141=LINE('',#10179,#2608);
#2142=LINE('',#10188,#2609);
#2143=LINE('',#10194,#2610);
#2144=LINE('',#10203,#2611);
#2145=LINE('',#10209,#2612);
#2146=LINE('',#10216,#2613);
#2147=LINE('',#10219,#2614);
#2148=LINE('',#10222,#2615);
#2149=LINE('',#10224,#2616);
#2150=LINE('',#10226,#2617);
#2151=LINE('',#10228,#2618);
#2152=LINE('',#10229,#2619);
#2153=LINE('',#10236,#2620);
#2154=LINE('',#10237,#2621);
#2155=LINE('',#10241,#2622);
#2156=LINE('',#10245,#2623);
#2157=LINE('',#10249,#2624);
#2158=LINE('',#10251,#2625);
#2159=LINE('',#10253,#2626);
#2160=LINE('',#10254,#2627);
#2161=LINE('',#10257,#2628);
#2162=LINE('',#10259,#2629);
#2163=LINE('',#10260,#2630);
#2164=LINE('',#10262,#2631);
#2165=LINE('',#10263,#2632);
#2166=LINE('',#10266,#2633);
#2167=LINE('',#10267,#2634);
#2168=LINE('',#10269,#2635);
#2169=LINE('',#10270,#2636);
#2170=LINE('',#10277,#2637);
#2171=LINE('',#10279,#2638);
#2172=LINE('',#10281,#2639);
#2173=LINE('',#10282,#2640);
#2174=LINE('',#10285,#2641);
#2175=LINE('',#10287,#2642);
#2176=LINE('',#10288,#2643);
#2177=LINE('',#10291,#2644);
#2178=LINE('',#10293,#2645);
#2179=LINE('',#10294,#2646);
#2180=LINE('',#10297,#2647);
#2181=LINE('',#10299,#2648);
#2182=LINE('',#10300,#2649);
#2183=LINE('',#10303,#2650);
#2184=LINE('',#10305,#2651);
#2185=LINE('',#10306,#2652);
#2186=LINE('',#10308,#2653);
#2187=LINE('',#10309,#2654);
#2188=LINE('',#10321,#2655);
#2189=LINE('',#10325,#2656);
#2190=LINE('',#10329,#2657);
#2191=LINE('',#10336,#2658);
#2192=LINE('',#10338,#2659);
#2193=LINE('',#10344,#2660);
#2194=LINE('',#10354,#2661);
#2195=LINE('',#10360,#2662);
#2196=LINE('',#10367,#2663);
#2197=LINE('',#10373,#2664);
#2198=LINE('',#10382,#2665);
#2199=LINE('',#10388,#2666);
#2200=LINE('',#10397,#2667);
#2201=LINE('',#10407,#2668);
#2202=LINE('',#10413,#2669);
#2203=LINE('',#10420,#2670);
#2204=LINE('',#10426,#2671);
#2205=LINE('',#10435,#2672);
#2206=LINE('',#10441,#2673);
#2207=LINE('',#10449,#2674);
#2208=LINE('',#10451,#2675);
#2209=LINE('',#10453,#2676);
#2210=LINE('',#10454,#2677);
#2211=LINE('',#10457,#2678);
#2212=LINE('',#10459,#2679);
#2213=LINE('',#10460,#2680);
#2214=LINE('',#10463,#2681);
#2215=LINE('',#10465,#2682);
#2216=LINE('',#10466,#2683);
#2217=LINE('',#10469,#2684);
#2218=LINE('',#10471,#2685);
#2219=LINE('',#10472,#2686);
#2220=LINE('',#10475,#2687);
#2221=LINE('',#10477,#2688);
#2222=LINE('',#10478,#2689);
#2223=LINE('',#10480,#2690);
#2224=LINE('',#10481,#2691);
#2225=LINE('',#10493,#2692);
#2226=LINE('',#10497,#2693);
#2227=LINE('',#10501,#2694);
#2228=LINE('',#10508,#2695);
#2229=LINE('',#10510,#2696);
#2230=LINE('',#10516,#2697);
#2231=LINE('',#10523,#2698);
#2232=LINE('',#10529,#2699);
#2233=LINE('',#10534,#2700);
#2234=LINE('',#10536,#2701);
#2235=LINE('',#10538,#2702);
#2236=LINE('',#10539,#2703);
#2237=LINE('',#10542,#2704);
#2238=LINE('',#10544,#2705);
#2239=LINE('',#10545,#2706);
#2240=LINE('',#10548,#2707);
#2241=LINE('',#10550,#2708);
#2242=LINE('',#10551,#2709);
#2243=LINE('',#10553,#2710);
#2244=LINE('',#10554,#2711);
#2245=LINE('',#10561,#2712);
#2246=LINE('',#10563,#2713);
#2247=LINE('',#10565,#2714);
#2248=LINE('',#10566,#2715);
#2249=LINE('',#10569,#2716);
#2250=LINE('',#10571,#2717);
#2251=LINE('',#10572,#2718);
#2252=LINE('',#10575,#2719);
#2253=LINE('',#10577,#2720);
#2254=LINE('',#10578,#2721);
#2255=LINE('',#10581,#2722);
#2256=LINE('',#10583,#2723);
#2257=LINE('',#10584,#2724);
#2258=LINE('',#10587,#2725);
#2259=LINE('',#10589,#2726);
#2260=LINE('',#10590,#2727);
#2261=LINE('',#10592,#2728);
#2262=LINE('',#10593,#2729);
#2263=LINE('',#10605,#2730);
#2264=LINE('',#10609,#2731);
#2265=LINE('',#10613,#2732);
#2266=LINE('',#10620,#2733);
#2267=LINE('',#10622,#2734);
#2268=LINE('',#10627,#2735);
#2269=LINE('',#10656,#2736);
#2270=LINE('',#10659,#2737);
#2271=LINE('',#10663,#2738);
#2272=LINE('',#10700,#2739);
#2273=LINE('',#10703,#2740);
#2274=LINE('',#10708,#2741);
#2275=LINE('',#10714,#2742);
#2276=LINE('',#10719,#2743);
#2277=LINE('',#10721,#2744);
#2278=LINE('',#10723,#2745);
#2279=LINE('',#10724,#2746);
#2280=LINE('',#10727,#2747);
#2281=LINE('',#10729,#2748);
#2282=LINE('',#10730,#2749);
#2283=LINE('',#10733,#2750);
#2284=LINE('',#10735,#2751);
#2285=LINE('',#10736,#2752);
#2286=LINE('',#10738,#2753);
#2287=LINE('',#10739,#2754);
#2288=LINE('',#10746,#2755);
#2289=LINE('',#10748,#2756);
#2290=LINE('',#10750,#2757);
#2291=LINE('',#10751,#2758);
#2292=LINE('',#10754,#2759);
#2293=LINE('',#10756,#2760);
#2294=LINE('',#10757,#2761);
#2295=LINE('',#10760,#2762);
#2296=LINE('',#10762,#2763);
#2297=LINE('',#10763,#2764);
#2298=LINE('',#10766,#2765);
#2299=LINE('',#10768,#2766);
#2300=LINE('',#10769,#2767);
#2301=LINE('',#10772,#2768);
#2302=LINE('',#10774,#2769);
#2303=LINE('',#10775,#2770);
#2304=LINE('',#10777,#2771);
#2305=LINE('',#10778,#2772);
#2306=LINE('',#10786,#2773);
#2307=LINE('',#10790,#2774);
#2308=LINE('',#10794,#2775);
#2309=LINE('',#10801,#2776);
#2310=LINE('',#10844,#2777);
#2311=LINE('',#10851,#2778);
#2312=LINE('',#10860,#2779);
#2313=LINE('',#10868,#2780);
#2314=LINE('',#10870,#2781);
#2315=LINE('',#10872,#2782);
#2316=LINE('',#10873,#2783);
#2317=LINE('',#10876,#2784);
#2318=LINE('',#10878,#2785);
#2319=LINE('',#10879,#2786);
#2320=LINE('',#10881,#2787);
#2321=LINE('',#10882,#2788);
#2322=LINE('',#10890,#2789);
#2323=LINE('',#10899,#2790);
#2324=LINE('',#10905,#2791);
#2325=LINE('',#10914,#2792);
#2326=LINE('',#10920,#2793);
#2327=LINE('',#10929,#2794);
#2328=LINE('',#10935,#2795);
#2329=LINE('',#11004,#2796);
#2330=LINE('',#11024,#2797);
#2331=LINE('',#11030,#2798);
#2332=LINE('',#11034,#2799);
#2333=LINE('',#11040,#2800);
#2334=LINE('',#11045,#2801);
#2335=LINE('',#11060,#2802);
#2336=LINE('',#11069,#2803);
#2337=LINE('',#11073,#2804);
#2338=LINE('',#11077,#2805);
#2339=LINE('',#11080,#2806);
#2340=LINE('',#11233,#2807);
#2341=LINE('',#11529,#2808);
#2342=LINE('',#11571,#2809);
#2343=LINE('',#11576,#2810);
#2344=LINE('',#11585,#2811);
#2345=LINE('',#11590,#2812);
#2346=LINE('',#11601,#2813);
#2347=LINE('',#11607,#2814);
#2348=LINE('',#11616,#2815);
#2349=LINE('',#11622,#2816);
#2350=LINE('',#11631,#2817);
#2351=LINE('',#11637,#2818);
#2352=VECTOR('',#7500,1.);
#2353=VECTOR('',#7501,1.);
#2354=VECTOR('',#7502,1.);
#2355=VECTOR('',#7503,1.);
#2356=VECTOR('',#7506,1.);
#2357=VECTOR('',#7507,1.);
#2358=VECTOR('',#7508,1.);
#2359=VECTOR('',#7511,1.);
#2360=VECTOR('',#7512,1.);
#2361=VECTOR('',#7513,1.);
#2362=VECTOR('',#7516,1.);
#2363=VECTOR('',#7517,1.);
#2364=VECTOR('',#7518,1.);
#2365=VECTOR('',#7521,1.);
#2366=VECTOR('',#7522,1.);
#2367=VECTOR('',#7523,1.);
#2368=VECTOR('',#7526,1.);
#2369=VECTOR('',#7527,1.);
#2370=VECTOR('',#7528,1.);
#2371=VECTOR('',#7531,1.);
#2372=VECTOR('',#7532,1.);
#2373=VECTOR('',#7533,1.);
#2374=VECTOR('',#7536,1.);
#2375=VECTOR('',#7537,1.);
#2376=VECTOR('',#7538,1.);
#2377=VECTOR('',#7541,1.);
#2378=VECTOR('',#7542,1.);
#2379=VECTOR('',#7543,1.);
#2380=VECTOR('',#7546,1.);
#2381=VECTOR('',#7547,1.);
#2382=VECTOR('',#7548,1.);
#2383=VECTOR('',#7549,1.);
#2384=VECTOR('',#7552,1.);
#2385=VECTOR('',#7553,1.);
#2386=VECTOR('',#7554,1.);
#2387=VECTOR('',#7557,1.);
#2388=VECTOR('',#7558,1.);
#2389=VECTOR('',#7559,1.);
#2390=VECTOR('',#7562,1.);
#2391=VECTOR('',#7563,1.);
#2392=VECTOR('',#7564,1.);
#2393=VECTOR('',#7567,1.);
#2394=VECTOR('',#7568,1.);
#2395=VECTOR('',#7569,1.);
#2396=VECTOR('',#7572,1.);
#2397=VECTOR('',#7573,1.);
#2398=VECTOR('',#7574,1.);
#2399=VECTOR('',#7577,1.);
#2400=VECTOR('',#7578,1.);
#2401=VECTOR('',#7579,1.);
#2402=VECTOR('',#7582,1.);
#2403=VECTOR('',#7583,1.);
#2404=VECTOR('',#7584,1.);
#2405=VECTOR('',#7587,1.);
#2406=VECTOR('',#7588,1.);
#2407=VECTOR('',#7589,1.);
#2408=VECTOR('',#7592,1.);
#2409=VECTOR('',#7593,1.);
#2410=VECTOR('',#7594,1.);
#2411=VECTOR('',#7595,1.);
#2412=VECTOR('',#7598,1.);
#2413=VECTOR('',#7599,1.);
#2414=VECTOR('',#7600,1.);
#2415=VECTOR('',#7603,1.);
#2416=VECTOR('',#7604,1.);
#2417=VECTOR('',#7605,1.);
#2418=VECTOR('',#7608,1.);
#2419=VECTOR('',#7609,1.);
#2420=VECTOR('',#7610,1.);
#2421=VECTOR('',#7613,1.);
#2422=VECTOR('',#7614,1.);
#2423=VECTOR('',#7615,1.);
#2424=VECTOR('',#7618,1.);
#2425=VECTOR('',#7619,1.);
#2426=VECTOR('',#7620,1.);
#2427=VECTOR('',#7623,1.);
#2428=VECTOR('',#7624,1.);
#2429=VECTOR('',#7625,1.);
#2430=VECTOR('',#7628,1.);
#2431=VECTOR('',#7629,1.);
#2432=VECTOR('',#7630,1.);
#2433=VECTOR('',#7633,1.);
#2434=VECTOR('',#7634,1.);
#2435=VECTOR('',#7635,1.);
#2436=VECTOR('',#7638,1.);
#2437=VECTOR('',#7639,1.);
#2438=VECTOR('',#7640,1.);
#2439=VECTOR('',#7641,1.);
#2440=VECTOR('',#7644,1.);
#2441=VECTOR('',#7645,1.);
#2442=VECTOR('',#7646,1.);
#2443=VECTOR('',#7649,1.);
#2444=VECTOR('',#7650,1.);
#2445=VECTOR('',#7651,1.);
#2446=VECTOR('',#7654,1.);
#2447=VECTOR('',#7655,1.);
#2448=VECTOR('',#7656,1.);
#2449=VECTOR('',#7659,1.);
#2450=VECTOR('',#7660,1.);
#2451=VECTOR('',#7661,1.);
#2452=VECTOR('',#7664,1.);
#2453=VECTOR('',#7665,1.);
#2454=VECTOR('',#7666,1.);
#2455=VECTOR('',#7669,1.);
#2456=VECTOR('',#7670,1.);
#2457=VECTOR('',#7671,1.);
#2458=VECTOR('',#7674,1.);
#2459=VECTOR('',#7675,1.);
#2460=VECTOR('',#7676,1.);
#2461=VECTOR('',#7679,1.);
#2462=VECTOR('',#7680,1.);
#2463=VECTOR('',#7681,1.);
#2464=VECTOR('',#7686,0.21);
#2465=VECTOR('',#7691,1.);
#2466=VECTOR('',#7692,1.);
#2467=VECTOR('',#7693,1.);
#2468=VECTOR('',#7696,1.);
#2469=VECTOR('',#7697,1.);
#2470=VECTOR('',#7698,1.);
#2471=VECTOR('',#7701,1.);
#2472=VECTOR('',#7702,1.);
#2473=VECTOR('',#7705,1.);
#2474=VECTOR('',#7706,1.);
#2475=VECTOR('',#7707,1.);
#2476=VECTOR('',#7710,1.);
#2477=VECTOR('',#7711,1.);
#2478=VECTOR('',#7714,1.);
#2479=VECTOR('',#7715,1.);
#2480=VECTOR('',#7716,1.);
#2481=VECTOR('',#7719,1.);
#2482=VECTOR('',#7720,1.);
#2483=VECTOR('',#7723,1.);
#2484=VECTOR('',#7724,1.);
#2485=VECTOR('',#7735,0.21);
#2486=VECTOR('',#7742,0.21);
#2487=VECTOR('',#7749,0.25);
#2488=VECTOR('',#7756,0.25);
#2489=VECTOR('',#7763,0.25);
#2490=VECTOR('',#7770,0.25);
#2491=VECTOR('',#7777,0.275);
#2492=VECTOR('',#7784,0.275);
#2493=VECTOR('',#7791,0.275);
#2494=VECTOR('',#7798,0.275);
#2495=VECTOR('',#7805,0.275);
#2496=VECTOR('',#7812,0.275);
#2497=VECTOR('',#7817,1.);
#2498=VECTOR('',#7818,1.);
#2499=VECTOR('',#7819,1.);
#2500=VECTOR('',#7820,1.);
#2501=VECTOR('',#7823,1.);
#2502=VECTOR('',#7824,1.);
#2503=VECTOR('',#7825,1.);
#2504=VECTOR('',#7828,1.);
#2505=VECTOR('',#7829,1.);
#2506=VECTOR('',#7830,1.);
#2507=VECTOR('',#7833,1.);
#2508=VECTOR('',#7834,1.);
#2509=VECTOR('',#7843,1.);
#2510=VECTOR('',#7844,1.);
#2511=VECTOR('',#7845,1.);
#2512=VECTOR('',#7846,1.);
#2513=VECTOR('',#7849,1.);
#2514=VECTOR('',#7850,1.);
#2515=VECTOR('',#7851,1.);
#2516=VECTOR('',#7854,1.);
#2517=VECTOR('',#7855,1.);
#2518=VECTOR('',#7856,1.);
#2519=VECTOR('',#7861,1.);
#2520=VECTOR('',#7862,1.);
#2521=VECTOR('',#7863,1.);
#2522=VECTOR('',#7864,1.);
#2523=VECTOR('',#7865,1.);
#2524=VECTOR('',#7866,1.);
#2525=VECTOR('',#7867,1.);
#2526=VECTOR('',#7870,1.);
#2527=VECTOR('',#7871,1.);
#2528=VECTOR('',#7874,1.);
#2529=VECTOR('',#7875,1.);
#2530=VECTOR('',#7878,1.);
#2531=VECTOR('',#7879,1.);
#2532=VECTOR('',#7880,1.);
#2533=VECTOR('',#7881,1.);
#2534=VECTOR('',#7882,1.);
#2535=VECTOR('',#7885,1.);
#2536=VECTOR('',#7888,1.);
#2537=VECTOR('',#7891,1.);
#2538=VECTOR('',#7896,0.21);
#2539=VECTOR('',#7905,1.);
#2540=VECTOR('',#7908,1.);
#2541=VECTOR('',#7911,1.);
#2542=VECTOR('',#7920,0.275);
#2543=VECTOR('',#7925,0.265);
#2544=VECTOR('',#7934,0.5);
#2545=VECTOR('',#7943,1.);
#2546=VECTOR('',#7944,1.);
#2547=VECTOR('',#7945,1.);
#2548=VECTOR('',#7946,1.);
#2549=VECTOR('',#7949,1.);
#2550=VECTOR('',#7950,1.);
#2551=VECTOR('',#7951,1.);
#2552=VECTOR('',#7954,1.);
#2553=VECTOR('',#7955,1.);
#2554=VECTOR('',#7956,1.);
#2555=VECTOR('',#7959,1.);
#2556=VECTOR('',#7960,1.);
#2557=VECTOR('',#7969,1.);
#2558=VECTOR('',#7970,1.);
#2559=VECTOR('',#7971,1.);
#2560=VECTOR('',#7972,1.);
#2561=VECTOR('',#7975,1.);
#2562=VECTOR('',#7976,1.);
#2563=VECTOR('',#7977,1.);
#2564=VECTOR('',#7980,1.);
#2565=VECTOR('',#7981,1.);
#2566=VECTOR('',#7982,1.);
#2567=VECTOR('',#7985,1.);
#2568=VECTOR('',#7986,1.);
#2569=VECTOR('',#7997,0.33);
#2570=VECTOR('',#8004,0.33);
#2571=VECTOR('',#8011,1.);
#2572=VECTOR('',#8014,1.);
#2573=VECTOR('',#8017,1.);
#2574=VECTOR('',#8018,1.);
#2575=VECTOR('',#8019,1.);
#2576=VECTOR('',#8020,1.);
#2577=VECTOR('',#8021,1.);
#2578=VECTOR('',#8028,1.);
#2579=VECTOR('',#8029,1.);
#2580=VECTOR('',#8034,0.5);
#2581=VECTOR('',#8039,0.5);
#2582=VECTOR('',#8042,1.);
#2583=VECTOR('',#8043,1.);
#2584=VECTOR('',#8044,1.);
#2585=VECTOR('',#8045,1.);
#2586=VECTOR('',#8048,1.);
#2587=VECTOR('',#8049,1.);
#2588=VECTOR('',#8050,1.);
#2589=VECTOR('',#8053,1.);
#2590=VECTOR('',#8054,1.);
#2591=VECTOR('',#8057,1.);
#2592=VECTOR('',#8058,1.);
#2593=VECTOR('',#8061,1.);
#2594=VECTOR('',#8062,1.);
#2595=VECTOR('',#8073,0.165);
#2596=VECTOR('',#8086,0.8);
#2597=VECTOR('',#8095,0.5);
#2598=VECTOR('',#8104,0.505);
#2599=VECTOR('',#8111,0.7);
#2600=VECTOR('',#8124,0.505);
#2601=VECTOR('',#8131,0.7);
#2602=VECTOR('',#8144,0.225);
#2603=VECTOR('',#8151,0.8);
#2604=VECTOR('',#8164,0.165);
#2605=VECTOR('',#8177,0.8);
#2606=VECTOR('',#8186,0.5);
#2607=VECTOR('',#8195,0.505);
#2608=VECTOR('',#8202,0.7);
#2609=VECTOR('',#8215,0.225);
#2610=VECTOR('',#8222,0.8);
#2611=VECTOR('',#8235,0.33);
#2612=VECTOR('',#8242,0.33);
#2613=VECTOR('',#8249,1.);
#2614=VECTOR('',#8252,1.);
#2615=VECTOR('',#8255,1.);
#2616=VECTOR('',#8256,1.);
#2617=VECTOR('',#8257,1.);
#2618=VECTOR('',#8258,1.);
#2619=VECTOR('',#8259,1.);
#2620=VECTOR('',#8266,1.);
#2621=VECTOR('',#8267,1.);
#2622=VECTOR('',#8272,0.5);
#2623=VECTOR('',#8277,0.5);
#2624=VECTOR('',#8280,1.);
#2625=VECTOR('',#8281,1.);
#2626=VECTOR('',#8282,1.);
#2627=VECTOR('',#8283,1.);
#2628=VECTOR('',#8286,1.);
#2629=VECTOR('',#8287,1.);
#2630=VECTOR('',#8288,1.);
#2631=VECTOR('',#8291,1.);
#2632=VECTOR('',#8292,1.);
#2633=VECTOR('',#8295,1.);
#2634=VECTOR('',#8296,1.);
#2635=VECTOR('',#8299,1.);
#2636=VECTOR('',#8300,1.);
#2637=VECTOR('',#8309,1.);
#2638=VECTOR('',#8310,1.);
#2639=VECTOR('',#8311,1.);
#2640=VECTOR('',#8312,1.);
#2641=VECTOR('',#8315,1.);
#2642=VECTOR('',#8316,1.);
#2643=VECTOR('',#8317,1.);
#2644=VECTOR('',#8320,1.);
#2645=VECTOR('',#8321,1.);
#2646=VECTOR('',#8322,1.);
#2647=VECTOR('',#8325,1.);
#2648=VECTOR('',#8326,1.);
#2649=VECTOR('',#8327,1.);
#2650=VECTOR('',#8330,1.);
#2651=VECTOR('',#8331,1.);
#2652=VECTOR('',#8332,1.);
#2653=VECTOR('',#8335,1.);
#2654=VECTOR('',#8336,1.);
#2655=VECTOR('',#8353,0.475);
#2656=VECTOR('',#8358,0.5);
#2657=VECTOR('',#8363,0.485);
#2658=VECTOR('',#8372,0.31);
#2659=VECTOR('',#8375,0.3);
#2660=VECTOR('',#8382,0.165);
#2661=VECTOR('',#8395,0.8);
#2662=VECTOR('',#8404,0.5);
#2663=VECTOR('',#8413,0.505);
#2664=VECTOR('',#8420,0.7);
#2665=VECTOR('',#8433,0.225);
#2666=VECTOR('',#8440,0.8);
#2667=VECTOR('',#8453,0.165);
#2668=VECTOR('',#8466,0.8);
#2669=VECTOR('',#8475,0.5);
#2670=VECTOR('',#8484,0.505);
#2671=VECTOR('',#8491,0.7);
#2672=VECTOR('',#8504,0.225);
#2673=VECTOR('',#8511,0.8);
#2674=VECTOR('',#8522,1.);
#2675=VECTOR('',#8523,1.);
#2676=VECTOR('',#8524,1.);
#2677=VECTOR('',#8525,1.);
#2678=VECTOR('',#8528,1.);
#2679=VECTOR('',#8529,1.);
#2680=VECTOR('',#8530,1.);
#2681=VECTOR('',#8533,1.);
#2682=VECTOR('',#8534,1.);
#2683=VECTOR('',#8535,1.);
#2684=VECTOR('',#8538,1.);
#2685=VECTOR('',#8539,1.);
#2686=VECTOR('',#8540,1.);
#2687=VECTOR('',#8543,1.);
#2688=VECTOR('',#8544,1.);
#2689=VECTOR('',#8545,1.);
#2690=VECTOR('',#8548,1.);
#2691=VECTOR('',#8549,1.);
#2692=VECTOR('',#8566,0.325);
#2693=VECTOR('',#8571,0.35);
#2694=VECTOR('',#8576,0.335);
#2695=VECTOR('',#8585,0.21);
#2696=VECTOR('',#8588,0.2);
#2697=VECTOR('',#8595,0.6);
#2698=VECTOR('',#8604,0.275);
#2699=VECTOR('',#8611,0.275);
#2700=VECTOR('',#8616,1.);
#2701=VECTOR('',#8617,1.);
#2702=VECTOR('',#8618,1.);
#2703=VECTOR('',#8619,1.);
#2704=VECTOR('',#8622,1.);
#2705=VECTOR('',#8623,1.);
#2706=VECTOR('',#8624,1.);
#2707=VECTOR('',#8627,1.);
#2708=VECTOR('',#8628,1.);
#2709=VECTOR('',#8629,1.);
#2710=VECTOR('',#8632,1.);
#2711=VECTOR('',#8633,1.);
#2712=VECTOR('',#8642,1.);
#2713=VECTOR('',#8643,1.);
#2714=VECTOR('',#8644,1.);
#2715=VECTOR('',#8645,1.);
#2716=VECTOR('',#8648,1.);
#2717=VECTOR('',#8649,1.);
#2718=VECTOR('',#8650,1.);
#2719=VECTOR('',#8653,1.);
#2720=VECTOR('',#8654,1.);
#2721=VECTOR('',#8655,1.);
#2722=VECTOR('',#8658,1.);
#2723=VECTOR('',#8659,1.);
#2724=VECTOR('',#8660,1.);
#2725=VECTOR('',#8663,1.);
#2726=VECTOR('',#8664,1.);
#2727=VECTOR('',#8665,1.);
#2728=VECTOR('',#8668,1.);
#2729=VECTOR('',#8669,1.);
#2730=VECTOR('',#8686,0.4);
#2731=VECTOR('',#8691,0.425);
#2732=VECTOR('',#8696,0.41);
#2733=VECTOR('',#8705,0.26);
#2734=VECTOR('',#8708,0.25);
#2735=VECTOR('',#8713,1.);
#2736=VECTOR('',#8722,0.21);
#2737=VECTOR('',#8727,1.);
#2738=VECTOR('',#8730,1.);
#2739=VECTOR('',#8739,0.21);
#2740=VECTOR('',#8744,1.);
#2741=VECTOR('',#8749,0.4);
#2742=VECTOR('',#8756,0.605000000000001);
#2743=VECTOR('',#8761,1.);
#2744=VECTOR('',#8762,1.);
#2745=VECTOR('',#8763,1.);
#2746=VECTOR('',#8764,1.);
#2747=VECTOR('',#8767,1.);
#2748=VECTOR('',#8768,1.);
#2749=VECTOR('',#8769,1.);
#2750=VECTOR('',#8772,1.);
#2751=VECTOR('',#8773,1.);
#2752=VECTOR('',#8774,1.);
#2753=VECTOR('',#8777,1.);
#2754=VECTOR('',#8778,1.);
#2755=VECTOR('',#8787,1.);
#2756=VECTOR('',#8788,1.);
#2757=VECTOR('',#8789,1.);
#2758=VECTOR('',#8790,1.);
#2759=VECTOR('',#8793,1.);
#2760=VECTOR('',#8794,1.);
#2761=VECTOR('',#8795,1.);
#2762=VECTOR('',#8798,1.);
#2763=VECTOR('',#8799,1.);
#2764=VECTOR('',#8800,1.);
#2765=VECTOR('',#8803,1.);
#2766=VECTOR('',#8804,1.);
#2767=VECTOR('',#8805,1.);
#2768=VECTOR('',#8808,1.);
#2769=VECTOR('',#8809,1.);
#2770=VECTOR('',#8810,1.);
#2771=VECTOR('',#8813,1.);
#2772=VECTOR('',#8814,1.);
#2773=VECTOR('',#8825,0.235);
#2774=VECTOR('',#8830,0.25);
#2775=VECTOR('',#8835,0.2125);
#2776=VECTOR('',#8844,0.15);
#2777=VECTOR('',#8851,0.4);
#2778=VECTOR('',#8860,1.8);
#2779=VECTOR('',#8873,1.6);
#2780=VECTOR('',#8884,1.);
#2781=VECTOR('',#8885,1.);
#2782=VECTOR('',#8886,1.);
#2783=VECTOR('',#8887,1.);
#2784=VECTOR('',#8890,1.);
#2785=VECTOR('',#8891,1.);
#2786=VECTOR('',#8892,1.);
#2787=VECTOR('',#8895,1.);
#2788=VECTOR('',#8896,1.);
#2789=VECTOR('',#8907,0.15);
#2790=VECTOR('',#8920,0.505);
#2791=VECTOR('',#8927,0.7);
#2792=VECTOR('',#8940,0.505);
#2793=VECTOR('',#8947,0.7);
#2794=VECTOR('',#8960,0.505);
#2795=VECTOR('',#8967,0.7);
#2796=VECTOR('',#9100,1.);
#2797=VECTOR('',#9129,0.976185);
#2798=VECTOR('',#9136,0.5);
#2799=VECTOR('',#9141,0.53);
#2800=VECTOR('',#9150,0.976185);
#2801=VECTOR('',#9157,0.53);
#2802=VECTOR('',#9176,1.023815);
#2803=VECTOR('',#9187,1.47);
#2804=VECTOR('',#9192,1.5);
#2805=VECTOR('',#9197,1.47);
#2806=VECTOR('',#9202,1.023815);
#2807=VECTOR('',#9253,1.019052);
#2808=VECTOR('',#9330,0.980948);
#2809=VECTOR('',#9359,1.013815);
#2810=VECTOR('',#9366,0.991185);
#2811=VECTOR('',#9377,1.013815);
#2812=VECTOR('',#9384,0.991185);
#2813=VECTOR('',#9401,1.5);
#2814=VECTOR('',#9408,1.8);
#2815=VECTOR('',#9421,1.1);
#2816=VECTOR('',#9428,1.8);
#2817=VECTOR('',#9441,1.1);
#2818=VECTOR('',#9448,1.8);
#2819=VERTEX_POINT('',#9479);
#2820=VERTEX_POINT('',#9480);
#2821=VERTEX_POINT('',#9482);
#2822=VERTEX_POINT('',#9484);
#2823=VERTEX_POINT('',#9488);
#2824=VERTEX_POINT('',#9490);
#2825=VERTEX_POINT('',#9494);
#2826=VERTEX_POINT('',#9496);
#2827=VERTEX_POINT('',#9500);
#2828=VERTEX_POINT('',#9502);
#2829=VERTEX_POINT('',#9506);
#2830=VERTEX_POINT('',#9508);
#2831=VERTEX_POINT('',#9512);
#2832=VERTEX_POINT('',#9514);
#2833=VERTEX_POINT('',#9518);
#2834=VERTEX_POINT('',#9520);
#2835=VERTEX_POINT('',#9524);
#2836=VERTEX_POINT('',#9526);
#2837=VERTEX_POINT('',#9530);
#2838=VERTEX_POINT('',#9532);
#2839=VERTEX_POINT('',#9536);
#2840=VERTEX_POINT('',#9537);
#2841=VERTEX_POINT('',#9539);
#2842=VERTEX_POINT('',#9541);
#2843=VERTEX_POINT('',#9545);
#2844=VERTEX_POINT('',#9547);
#2845=VERTEX_POINT('',#9551);
#2846=VERTEX_POINT('',#9553);
#2847=VERTEX_POINT('',#9557);
#2848=VERTEX_POINT('',#9559);
#2849=VERTEX_POINT('',#9563);
#2850=VERTEX_POINT('',#9565);
#2851=VERTEX_POINT('',#9569);
#2852=VERTEX_POINT('',#9571);
#2853=VERTEX_POINT('',#9575);
#2854=VERTEX_POINT('',#9577);
#2855=VERTEX_POINT('',#9581);
#2856=VERTEX_POINT('',#9583);
#2857=VERTEX_POINT('',#9587);
#2858=VERTEX_POINT('',#9589);
#2859=VERTEX_POINT('',#9593);
#2860=VERTEX_POINT('',#9594);
#2861=VERTEX_POINT('',#9596);
#2862=VERTEX_POINT('',#9598);
#2863=VERTEX_POINT('',#9602);
#2864=VERTEX_POINT('',#9604);
#2865=VERTEX_POINT('',#9608);
#2866=VERTEX_POINT('',#9610);
#2867=VERTEX_POINT('',#9614);
#2868=VERTEX_POINT('',#9616);
#2869=VERTEX_POINT('',#9620);
#2870=VERTEX_POINT('',#9622);
#2871=VERTEX_POINT('',#9626);
#2872=VERTEX_POINT('',#9628);
#2873=VERTEX_POINT('',#9632);
#2874=VERTEX_POINT('',#9634);
#2875=VERTEX_POINT('',#9638);
#2876=VERTEX_POINT('',#9640);
#2877=VERTEX_POINT('',#9644);
#2878=VERTEX_POINT('',#9646);
#2879=VERTEX_POINT('',#9650);
#2880=VERTEX_POINT('',#9651);
#2881=VERTEX_POINT('',#9653);
#2882=VERTEX_POINT('',#9655);
#2883=VERTEX_POINT('',#9659);
#2884=VERTEX_POINT('',#9661);
#2885=VERTEX_POINT('',#9665);
#2886=VERTEX_POINT('',#9667);
#2887=VERTEX_POINT('',#9671);
#2888=VERTEX_POINT('',#9673);
#2889=VERTEX_POINT('',#9677);
#2890=VERTEX_POINT('',#9679);
#2891=VERTEX_POINT('',#9683);
#2892=VERTEX_POINT('',#9685);
#2893=VERTEX_POINT('',#9689);
#2894=VERTEX_POINT('',#9691);
#2895=VERTEX_POINT('',#9695);
#2896=VERTEX_POINT('',#9697);
#2897=VERTEX_POINT('',#9701);
#2898=VERTEX_POINT('',#9703);
#2899=VERTEX_POINT('',#9707);
#2900=VERTEX_POINT('',#9709);
#2901=VERTEX_POINT('',#9713);
#2902=VERTEX_POINT('',#9715);
#2903=VERTEX_POINT('',#9719);
#2904=VERTEX_POINT('',#9721);
#2905=VERTEX_POINT('',#9728);
#2906=VERTEX_POINT('',#9730);
#2907=VERTEX_POINT('',#9737);
#2908=VERTEX_POINT('',#9739);
#2909=VERTEX_POINT('',#9752);
#2910=VERTEX_POINT('',#9754);
#2911=VERTEX_POINT('',#9758);
#2912=VERTEX_POINT('',#9760);
#2913=VERTEX_POINT('',#9764);
#2914=VERTEX_POINT('',#9766);
#2915=VERTEX_POINT('',#9770);
#2916=VERTEX_POINT('',#9772);
#2917=VERTEX_POINT('',#9776);
#2918=VERTEX_POINT('',#9778);
#2919=VERTEX_POINT('',#9782);
#2920=VERTEX_POINT('',#9784);
#2921=VERTEX_POINT('',#9788);
#2922=VERTEX_POINT('',#9790);
#2923=VERTEX_POINT('',#9794);
#2924=VERTEX_POINT('',#9796);
#2925=VERTEX_POINT('',#9800);
#2926=VERTEX_POINT('',#9802);
#2927=VERTEX_POINT('',#9806);
#2928=VERTEX_POINT('',#9808);
#2929=VERTEX_POINT('',#9812);
#2930=VERTEX_POINT('',#9814);
#2931=VERTEX_POINT('',#9818);
#2932=VERTEX_POINT('',#9820);
#2933=VERTEX_POINT('',#9824);
#2934=VERTEX_POINT('',#9825);
#2935=VERTEX_POINT('',#9827);
#2936=VERTEX_POINT('',#9829);
#2937=VERTEX_POINT('',#9833);
#2938=VERTEX_POINT('',#9835);
#2939=VERTEX_POINT('',#9839);
#2940=VERTEX_POINT('',#9841);
#2941=VERTEX_POINT('',#9851);
#2942=VERTEX_POINT('',#9852);
#2943=VERTEX_POINT('',#9854);
#2944=VERTEX_POINT('',#9856);
#2945=VERTEX_POINT('',#9860);
#2946=VERTEX_POINT('',#9862);
#2947=VERTEX_POINT('',#9866);
#2948=VERTEX_POINT('',#9868);
#2949=VERTEX_POINT('',#9871);
#2950=VERTEX_POINT('',#9874);
#2951=VERTEX_POINT('',#9876);
#2952=VERTEX_POINT('',#9878);
#2953=VERTEX_POINT('',#9880);
#2954=VERTEX_POINT('',#9882);
#2955=VERTEX_POINT('',#9884);
#2956=VERTEX_POINT('',#9888);
#2957=VERTEX_POINT('',#9892);
#2958=VERTEX_POINT('',#9896);
#2959=VERTEX_POINT('',#9898);
#2960=VERTEX_POINT('',#9900);
#2961=VERTEX_POINT('',#9902);
#2962=VERTEX_POINT('',#9908);
#2963=VERTEX_POINT('',#9910);
#2964=VERTEX_POINT('',#9914);
#2965=VERTEX_POINT('',#9917);
#2966=VERTEX_POINT('',#9919);
#2967=VERTEX_POINT('',#9931);
#2968=VERTEX_POINT('',#9933);
#2969=VERTEX_POINT('',#9937);
#2970=VERTEX_POINT('',#9941);
#2971=VERTEX_POINT('',#9944);
#2972=VERTEX_POINT('',#9950);
#2973=VERTEX_POINT('',#9951);
#2974=VERTEX_POINT('',#9953);
#2975=VERTEX_POINT('',#9955);
#2976=VERTEX_POINT('',#9959);
#2977=VERTEX_POINT('',#9961);
#2978=VERTEX_POINT('',#9965);
#2979=VERTEX_POINT('',#9967);
#2980=VERTEX_POINT('',#9977);
#2981=VERTEX_POINT('',#9978);
#2982=VERTEX_POINT('',#9980);
#2983=VERTEX_POINT('',#9982);
#2984=VERTEX_POINT('',#9986);
#2985=VERTEX_POINT('',#9988);
#2986=VERTEX_POINT('',#9992);
#2987=VERTEX_POINT('',#9994);
#2988=VERTEX_POINT('',#10004);
#2989=VERTEX_POINT('',#10006);
#2990=VERTEX_POINT('',#10010);
#2991=VERTEX_POINT('',#10012);
#2992=VERTEX_POINT('',#10016);
#2993=VERTEX_POINT('',#10017);
#2994=VERTEX_POINT('',#10019);
#2995=VERTEX_POINT('',#10021);
#2996=VERTEX_POINT('',#10025);
#2997=VERTEX_POINT('',#10027);
#2998=VERTEX_POINT('',#10029);
#2999=VERTEX_POINT('',#10031);
#3000=VERTEX_POINT('',#10034);
#3001=VERTEX_POINT('',#10036);
#3002=VERTEX_POINT('',#10039);
#3003=VERTEX_POINT('',#10043);
#3004=VERTEX_POINT('',#10047);
#3005=VERTEX_POINT('',#10051);
#3006=VERTEX_POINT('',#10052);
#3007=VERTEX_POINT('',#10054);
#3008=VERTEX_POINT('',#10056);
#3009=VERTEX_POINT('',#10060);
#3010=VERTEX_POINT('',#10062);
#3011=VERTEX_POINT('',#10069);
#3012=VERTEX_POINT('',#10079);
#3013=VERTEX_POINT('',#10081);
#3014=VERTEX_POINT('',#10086);
#3015=VERTEX_POINT('',#10088);
#3016=VERTEX_POINT('',#10091);
#3017=VERTEX_POINT('',#10096);
#3018=VERTEX_POINT('',#10102);
#3019=VERTEX_POINT('',#10104);
#3020=VERTEX_POINT('',#10108);
#3021=VERTEX_POINT('',#10110);
#3022=VERTEX_POINT('',#10117);
#3023=VERTEX_POINT('',#10119);
#3024=VERTEX_POINT('',#10123);
#3025=VERTEX_POINT('',#10125);
#3026=VERTEX_POINT('',#10132);
#3027=VERTEX_POINT('',#10134);
#3028=VERTEX_POINT('',#10138);
#3029=VERTEX_POINT('',#10140);
#3030=VERTEX_POINT('',#10147);
#3031=VERTEX_POINT('',#10149);
#3032=VERTEX_POINT('',#10154);
#3033=VERTEX_POINT('',#10156);
#3034=VERTEX_POINT('',#10159);
#3035=VERTEX_POINT('',#10164);
#3036=VERTEX_POINT('',#10170);
#3037=VERTEX_POINT('',#10172);
#3038=VERTEX_POINT('',#10176);
#3039=VERTEX_POINT('',#10178);
#3040=VERTEX_POINT('',#10185);
#3041=VERTEX_POINT('',#10187);
#3042=VERTEX_POINT('',#10191);
#3043=VERTEX_POINT('',#10193);
#3044=VERTEX_POINT('',#10200);
#3045=VERTEX_POINT('',#10202);
#3046=VERTEX_POINT('',#10206);
#3047=VERTEX_POINT('',#10208);
#3048=VERTEX_POINT('',#10212);
#3049=VERTEX_POINT('',#10213);
#3050=VERTEX_POINT('',#10215);
#3051=VERTEX_POINT('',#10217);
#3052=VERTEX_POINT('',#10221);
#3053=VERTEX_POINT('',#10223);
#3054=VERTEX_POINT('',#10225);
#3055=VERTEX_POINT('',#10227);
#3056=VERTEX_POINT('',#10230);
#3057=VERTEX_POINT('',#10232);
#3058=VERTEX_POINT('',#10235);
#3059=VERTEX_POINT('',#10239);
#3060=VERTEX_POINT('',#10243);
#3061=VERTEX_POINT('',#10247);
#3062=VERTEX_POINT('',#10248);
#3063=VERTEX_POINT('',#10250);
#3064=VERTEX_POINT('',#10252);
#3065=VERTEX_POINT('',#10256);
#3066=VERTEX_POINT('',#10258);
#3067=VERTEX_POINT('',#10265);
#3068=VERTEX_POINT('',#10275);
#3069=VERTEX_POINT('',#10276);
#3070=VERTEX_POINT('',#10278);
#3071=VERTEX_POINT('',#10280);
#3072=VERTEX_POINT('',#10284);
#3073=VERTEX_POINT('',#10286);
#3074=VERTEX_POINT('',#10290);
#3075=VERTEX_POINT('',#10292);
#3076=VERTEX_POINT('',#10296);
#3077=VERTEX_POINT('',#10298);
#3078=VERTEX_POINT('',#10302);
#3079=VERTEX_POINT('',#10304);
#3080=VERTEX_POINT('',#10313);
#3081=VERTEX_POINT('',#10316);
#3082=VERTEX_POINT('',#10319);
#3083=VERTEX_POINT('',#10323);
#3084=VERTEX_POINT('',#10327);
#3085=VERTEX_POINT('',#10331);
#3086=VERTEX_POINT('',#10334);
#3087=VERTEX_POINT('',#10341);
#3088=VERTEX_POINT('',#10343);
#3089=VERTEX_POINT('',#10348);
#3090=VERTEX_POINT('',#10350);
#3091=VERTEX_POINT('',#10353);
#3092=VERTEX_POINT('',#10358);
#3093=VERTEX_POINT('',#10364);
#3094=VERTEX_POINT('',#10366);
#3095=VERTEX_POINT('',#10370);
#3096=VERTEX_POINT('',#10372);
#3097=VERTEX_POINT('',#10379);
#3098=VERTEX_POINT('',#10381);
#3099=VERTEX_POINT('',#10385);
#3100=VERTEX_POINT('',#10387);
#3101=VERTEX_POINT('',#10394);
#3102=VERTEX_POINT('',#10396);
#3103=VERTEX_POINT('',#10401);
#3104=VERTEX_POINT('',#10403);
#3105=VERTEX_POINT('',#10406);
#3106=VERTEX_POINT('',#10411);
#3107=VERTEX_POINT('',#10417);
#3108=VERTEX_POINT('',#10419);
#3109=VERTEX_POINT('',#10423);
#3110=VERTEX_POINT('',#10425);
#3111=VERTEX_POINT('',#10432);
#3112=VERTEX_POINT('',#10434);
#3113=VERTEX_POINT('',#10438);
#3114=VERTEX_POINT('',#10440);
#3115=VERTEX_POINT('',#10447);
#3116=VERTEX_POINT('',#10448);
#3117=VERTEX_POINT('',#10450);
#3118=VERTEX_POINT('',#10452);
#3119=VERTEX_POINT('',#10456);
#3120=VERTEX_POINT('',#10458);
#3121=VERTEX_POINT('',#10462);
#3122=VERTEX_POINT('',#10464);
#3123=VERTEX_POINT('',#10468);
#3124=VERTEX_POINT('',#10470);
#3125=VERTEX_POINT('',#10474);
#3126=VERTEX_POINT('',#10476);
#3127=VERTEX_POINT('',#10485);
#3128=VERTEX_POINT('',#10488);
#3129=VERTEX_POINT('',#10491);
#3130=VERTEX_POINT('',#10495);
#3131=VERTEX_POINT('',#10499);
#3132=VERTEX_POINT('',#10503);
#3133=VERTEX_POINT('',#10506);
#3134=VERTEX_POINT('',#10513);
#3135=VERTEX_POINT('',#10515);
#3136=VERTEX_POINT('',#10520);
#3137=VERTEX_POINT('',#10522);
#3138=VERTEX_POINT('',#10526);
#3139=VERTEX_POINT('',#10528);
#3140=VERTEX_POINT('',#10532);
#3141=VERTEX_POINT('',#10533);
#3142=VERTEX_POINT('',#10535);
#3143=VERTEX_POINT('',#10537);
#3144=VERTEX_POINT('',#10541);
#3145=VERTEX_POINT('',#10543);
#3146=VERTEX_POINT('',#10547);
#3147=VERTEX_POINT('',#10549);
#3148=VERTEX_POINT('',#10559);
#3149=VERTEX_POINT('',#10560);
#3150=VERTEX_POINT('',#10562);
#3151=VERTEX_POINT('',#10564);
#3152=VERTEX_POINT('',#10568);
#3153=VERTEX_POINT('',#10570);
#3154=VERTEX_POINT('',#10574);
#3155=VERTEX_POINT('',#10576);
#3156=VERTEX_POINT('',#10580);
#3157=VERTEX_POINT('',#10582);
#3158=VERTEX_POINT('',#10586);
#3159=VERTEX_POINT('',#10588);
#3160=VERTEX_POINT('',#10597);
#3161=VERTEX_POINT('',#10600);
#3162=VERTEX_POINT('',#10603);
#3163=VERTEX_POINT('',#10607);
#3164=VERTEX_POINT('',#10611);
#3165=VERTEX_POINT('',#10615);
#3166=VERTEX_POINT('',#10618);
#3167=VERTEX_POINT('',#10625);
#3168=VERTEX_POINT('',#10626);
#3169=VERTEX_POINT('',#10628);
#3170=VERTEX_POINT('',#10632);
#3171=VERTEX_POINT('',#10643);
#3172=VERTEX_POINT('',#10655);
#3173=VERTEX_POINT('',#10661);
#3174=VERTEX_POINT('',#10662);
#3175=VERTEX_POINT('',#10664);
#3176=VERTEX_POINT('',#10668);
#3177=VERTEX_POINT('',#10683);
#3178=VERTEX_POINT('',#10699);
#3179=VERTEX_POINT('',#10705);
#3180=VERTEX_POINT('',#10707);
#3181=VERTEX_POINT('',#10711);
#3182=VERTEX_POINT('',#10713);
#3183=VERTEX_POINT('',#10717);
#3184=VERTEX_POINT('',#10718);
#3185=VERTEX_POINT('',#10720);
#3186=VERTEX_POINT('',#10722);
#3187=VERTEX_POINT('',#10726);
#3188=VERTEX_POINT('',#10728);
#3189=VERTEX_POINT('',#10732);
#3190=VERTEX_POINT('',#10734);
#3191=VERTEX_POINT('',#10744);
#3192=VERTEX_POINT('',#10745);
#3193=VERTEX_POINT('',#10747);
#3194=VERTEX_POINT('',#10749);
#3195=VERTEX_POINT('',#10753);
#3196=VERTEX_POINT('',#10755);
#3197=VERTEX_POINT('',#10759);
#3198=VERTEX_POINT('',#10761);
#3199=VERTEX_POINT('',#10765);
#3200=VERTEX_POINT('',#10767);
#3201=VERTEX_POINT('',#10771);
#3202=VERTEX_POINT('',#10773);
#3203=VERTEX_POINT('',#10781);
#3204=VERTEX_POINT('',#10784);
#3205=VERTEX_POINT('',#10788);
#3206=VERTEX_POINT('',#10792);
#3207=VERTEX_POINT('',#10798);
#3208=VERTEX_POINT('',#10800);
#3209=VERTEX_POINT('',#10805);
#3210=VERTEX_POINT('',#10806);
#3211=VERTEX_POINT('',#10843);
#3212=VERTEX_POINT('',#10848);
#3213=VERTEX_POINT('',#10850);
#3214=VERTEX_POINT('',#10857);
#3215=VERTEX_POINT('',#10859);
#3216=VERTEX_POINT('',#10866);
#3217=VERTEX_POINT('',#10867);
#3218=VERTEX_POINT('',#10869);
#3219=VERTEX_POINT('',#10871);
#3220=VERTEX_POINT('',#10875);
#3221=VERTEX_POINT('',#10877);
#3222=VERTEX_POINT('',#10887);
#3223=VERTEX_POINT('',#10889);
#3224=VERTEX_POINT('',#10896);
#3225=VERTEX_POINT('',#10898);
#3226=VERTEX_POINT('',#10902);
#3227=VERTEX_POINT('',#10904);
#3228=VERTEX_POINT('',#10911);
#3229=VERTEX_POINT('',#10913);
#3230=VERTEX_POINT('',#10917);
#3231=VERTEX_POINT('',#10919);
#3232=VERTEX_POINT('',#10926);
#3233=VERTEX_POINT('',#10928);
#3234=VERTEX_POINT('',#10932);
#3235=VERTEX_POINT('',#10934);
#3236=VERTEX_POINT('',#11001);
#3237=VERTEX_POINT('',#11003);
#3238=VERTEX_POINT('',#11013);
#3239=VERTEX_POINT('',#11014);
#3240=VERTEX_POINT('',#11017);
#3241=VERTEX_POINT('',#11019);
#3242=VERTEX_POINT('',#11023);
#3243=VERTEX_POINT('',#11027);
#3244=VERTEX_POINT('',#11029);
#3245=VERTEX_POINT('',#11033);
#3246=VERTEX_POINT('',#11038);
#3247=VERTEX_POINT('',#11042);
#3248=VERTEX_POINT('',#11048);
#3249=VERTEX_POINT('',#11049);
#3250=VERTEX_POINT('',#11052);
#3251=VERTEX_POINT('',#11054);
#3252=VERTEX_POINT('',#11058);
#3253=VERTEX_POINT('',#11062);
#3254=VERTEX_POINT('',#11064);
#3255=VERTEX_POINT('',#11067);
#3256=VERTEX_POINT('',#11071);
#3257=VERTEX_POINT('',#11075);
#3258=VERTEX_POINT('',#11083);
#3259=VERTEX_POINT('',#11084);
#3260=VERTEX_POINT('',#11087);
#3261=VERTEX_POINT('',#11088);
#3262=VERTEX_POINT('',#11091);
#3263=VERTEX_POINT('',#11092);
#3264=VERTEX_POINT('',#11095);
#3265=VERTEX_POINT('',#11096);
#3266=VERTEX_POINT('',#11099);
#3267=VERTEX_POINT('',#11100);
#3268=VERTEX_POINT('',#11103);
#3269=VERTEX_POINT('',#11104);
#3270=VERTEX_POINT('',#11107);
#3271=VERTEX_POINT('',#11108);
#3272=VERTEX_POINT('',#11111);
#3273=VERTEX_POINT('',#11112);
#3274=VERTEX_POINT('',#11116);
#3275=VERTEX_POINT('',#11117);
#3276=VERTEX_POINT('',#11140);
#3277=VERTEX_POINT('',#11142);
#3278=VERTEX_POINT('',#11167);
#3279=VERTEX_POINT('',#11169);
#3280=VERTEX_POINT('',#11192);
#3281=VERTEX_POINT('',#11194);
#3282=VERTEX_POINT('',#11217);
#3283=VERTEX_POINT('',#11219);
#3284=VERTEX_POINT('',#11232);
#3285=VERTEX_POINT('',#11235);
#3286=VERTEX_POINT('',#11248);
#3287=VERTEX_POINT('',#11250);
#3288=VERTEX_POINT('',#11273);
#3289=VERTEX_POINT('',#11275);
#3290=VERTEX_POINT('',#11298);
#3291=VERTEX_POINT('',#11300);
#3292=VERTEX_POINT('',#11323);
#3293=VERTEX_POINT('',#11325);
#3294=VERTEX_POINT('',#11350);
#3295=VERTEX_POINT('',#11354);
#3296=VERTEX_POINT('',#11379);
#3297=VERTEX_POINT('',#11383);
#3298=VERTEX_POINT('',#11408);
#3299=VERTEX_POINT('',#11412);
#3300=VERTEX_POINT('',#11413);
#3301=VERTEX_POINT('',#11440);
#3302=VERTEX_POINT('',#11444);
#3303=VERTEX_POINT('',#11469);
#3304=VERTEX_POINT('',#11473);
#3305=VERTEX_POINT('',#11498);
#3306=VERTEX_POINT('',#11502);
#3307=VERTEX_POINT('',#11527);
#3308=VERTEX_POINT('',#11530);
#3309=VERTEX_POINT('',#11532);
#3310=VERTEX_POINT('',#11564);
#3311=VERTEX_POINT('',#11566);
#3312=VERTEX_POINT('',#11569);
#3313=VERTEX_POINT('',#11573);
#3314=VERTEX_POINT('',#11578);
#3315=VERTEX_POINT('',#11580);
#3316=VERTEX_POINT('',#11583);
#3317=VERTEX_POINT('',#11587);
#3318=VERTEX_POINT('',#11598);
#3319=VERTEX_POINT('',#11600);
#3320=VERTEX_POINT('',#11604);
#3321=VERTEX_POINT('',#11606);
#3322=VERTEX_POINT('',#11613);
#3323=VERTEX_POINT('',#11615);
#3324=VERTEX_POINT('',#11619);
#3325=VERTEX_POINT('',#11621);
#3326=VERTEX_POINT('',#11628);
#3327=VERTEX_POINT('',#11630);
#3328=VERTEX_POINT('',#11634);
#3329=VERTEX_POINT('',#11636);
#3330=EDGE_CURVE('',#2819,#2820,#1885,.T.);
#3331=EDGE_CURVE('',#2819,#2821,#1886,.T.);
#3332=EDGE_CURVE('',#2822,#2821,#1887,.T.);
#3333=EDGE_CURVE('',#2820,#2822,#1888,.T.);
#3334=EDGE_CURVE('',#2823,#2819,#1889,.T.);
#3335=EDGE_CURVE('',#2823,#2824,#1890,.T.);
#3336=EDGE_CURVE('',#2821,#2824,#1891,.T.);
#3337=EDGE_CURVE('',#2825,#2823,#1892,.T.);
#3338=EDGE_CURVE('',#2825,#2826,#1893,.T.);
#3339=EDGE_CURVE('',#2824,#2826,#1894,.T.);
#3340=EDGE_CURVE('',#2827,#2825,#1895,.T.);
#3341=EDGE_CURVE('',#2827,#2828,#1896,.T.);
#3342=EDGE_CURVE('',#2826,#2828,#1897,.T.);
#3343=EDGE_CURVE('',#2829,#2827,#1898,.T.);
#3344=EDGE_CURVE('',#2829,#2830,#1899,.T.);
#3345=EDGE_CURVE('',#2828,#2830,#1900,.T.);
#3346=EDGE_CURVE('',#2831,#2829,#1901,.T.);
#3347=EDGE_CURVE('',#2831,#2832,#1902,.T.);
#3348=EDGE_CURVE('',#2830,#2832,#1903,.T.);
#3349=EDGE_CURVE('',#2833,#2831,#1904,.T.);
#3350=EDGE_CURVE('',#2833,#2834,#1905,.T.);
#3351=EDGE_CURVE('',#2832,#2834,#1906,.T.);
#3352=EDGE_CURVE('',#2835,#2833,#1907,.T.);
#3353=EDGE_CURVE('',#2835,#2836,#1908,.T.);
#3354=EDGE_CURVE('',#2834,#2836,#1909,.T.);
#3355=EDGE_CURVE('',#2837,#2835,#1910,.T.);
#3356=EDGE_CURVE('',#2838,#2837,#1911,.T.);
#3357=EDGE_CURVE('',#2836,#2838,#1912,.T.);
#3358=EDGE_CURVE('',#2839,#2840,#1913,.T.);
#3359=EDGE_CURVE('',#2839,#2841,#1914,.T.);
#3360=EDGE_CURVE('',#2842,#2841,#1915,.T.);
#3361=EDGE_CURVE('',#2840,#2842,#1916,.T.);
#3362=EDGE_CURVE('',#2843,#2839,#1917,.T.);
#3363=EDGE_CURVE('',#2843,#2844,#1918,.T.);
#3364=EDGE_CURVE('',#2841,#2844,#1919,.T.);
#3365=EDGE_CURVE('',#2845,#2843,#1920,.T.);
#3366=EDGE_CURVE('',#2845,#2846,#1921,.T.);
#3367=EDGE_CURVE('',#2844,#2846,#1922,.T.);
#3368=EDGE_CURVE('',#2847,#2845,#1923,.T.);
#3369=EDGE_CURVE('',#2847,#2848,#1924,.T.);
#3370=EDGE_CURVE('',#2846,#2848,#1925,.T.);
#3371=EDGE_CURVE('',#2849,#2847,#1926,.T.);
#3372=EDGE_CURVE('',#2849,#2850,#1927,.T.);
#3373=EDGE_CURVE('',#2848,#2850,#1928,.T.);
#3374=EDGE_CURVE('',#2851,#2849,#1929,.T.);
#3375=EDGE_CURVE('',#2851,#2852,#1930,.T.);
#3376=EDGE_CURVE('',#2850,#2852,#1931,.T.);
#3377=EDGE_CURVE('',#2853,#2851,#1932,.T.);
#3378=EDGE_CURVE('',#2853,#2854,#1933,.T.);
#3379=EDGE_CURVE('',#2852,#2854,#1934,.T.);
#3380=EDGE_CURVE('',#2855,#2853,#1935,.T.);
#3381=EDGE_CURVE('',#2855,#2856,#1936,.T.);
#3382=EDGE_CURVE('',#2854,#2856,#1937,.T.);
#3383=EDGE_CURVE('',#2857,#2855,#1938,.T.);
#3384=EDGE_CURVE('',#2858,#2857,#1939,.T.);
#3385=EDGE_CURVE('',#2856,#2858,#1940,.T.);
#3386=EDGE_CURVE('',#2859,#2860,#1941,.T.);
#3387=EDGE_CURVE('',#2859,#2861,#1942,.T.);
#3388=EDGE_CURVE('',#2862,#2861,#1943,.T.);
#3389=EDGE_CURVE('',#2860,#2862,#1944,.T.);
#3390=EDGE_CURVE('',#2863,#2859,#1945,.T.);
#3391=EDGE_CURVE('',#2863,#2864,#1946,.T.);
#3392=EDGE_CURVE('',#2861,#2864,#1947,.T.);
#3393=EDGE_CURVE('',#2865,#2863,#1948,.T.);
#3394=EDGE_CURVE('',#2865,#2866,#1949,.T.);
#3395=EDGE_CURVE('',#2864,#2866,#1950,.T.);
#3396=EDGE_CURVE('',#2867,#2865,#1951,.T.);
#3397=EDGE_CURVE('',#2867,#2868,#1952,.T.);
#3398=EDGE_CURVE('',#2866,#2868,#1953,.T.);
#3399=EDGE_CURVE('',#2869,#2867,#1954,.T.);
#3400=EDGE_CURVE('',#2869,#2870,#1955,.T.);
#3401=EDGE_CURVE('',#2868,#2870,#1956,.T.);
#3402=EDGE_CURVE('',#2871,#2869,#1957,.T.);
#3403=EDGE_CURVE('',#2871,#2872,#1958,.T.);
#3404=EDGE_CURVE('',#2870,#2872,#1959,.T.);
#3405=EDGE_CURVE('',#2873,#2871,#1960,.T.);
#3406=EDGE_CURVE('',#2873,#2874,#1961,.T.);
#3407=EDGE_CURVE('',#2872,#2874,#1962,.T.);
#3408=EDGE_CURVE('',#2875,#2873,#1963,.T.);
#3409=EDGE_CURVE('',#2875,#2876,#1964,.T.);
#3410=EDGE_CURVE('',#2874,#2876,#1965,.T.);
#3411=EDGE_CURVE('',#2877,#2875,#1966,.T.);
#3412=EDGE_CURVE('',#2878,#2877,#1967,.T.);
#3413=EDGE_CURVE('',#2876,#2878,#1968,.T.);
#3414=EDGE_CURVE('',#2879,#2880,#1969,.T.);
#3415=EDGE_CURVE('',#2879,#2881,#1970,.T.);
#3416=EDGE_CURVE('',#2882,#2881,#1971,.T.);
#3417=EDGE_CURVE('',#2880,#2882,#1972,.T.);
#3418=EDGE_CURVE('',#2883,#2879,#1973,.T.);
#3419=EDGE_CURVE('',#2883,#2884,#1974,.T.);
#3420=EDGE_CURVE('',#2881,#2884,#1975,.T.);
#3421=EDGE_CURVE('',#2885,#2883,#1976,.T.);
#3422=EDGE_CURVE('',#2885,#2886,#1977,.T.);
#3423=EDGE_CURVE('',#2884,#2886,#1978,.T.);
#3424=EDGE_CURVE('',#2887,#2885,#1979,.T.);
#3425=EDGE_CURVE('',#2887,#2888,#1980,.T.);
#3426=EDGE_CURVE('',#2886,#2888,#1981,.T.);
#3427=EDGE_CURVE('',#2889,#2887,#1982,.T.);
#3428=EDGE_CURVE('',#2889,#2890,#1983,.T.);
#3429=EDGE_CURVE('',#2888,#2890,#1984,.T.);
#3430=EDGE_CURVE('',#2891,#2889,#1985,.T.);
#3431=EDGE_CURVE('',#2891,#2892,#1986,.T.);
#3432=EDGE_CURVE('',#2890,#2892,#1987,.T.);
#3433=EDGE_CURVE('',#2893,#2891,#1988,.T.);
#3434=EDGE_CURVE('',#2893,#2894,#1989,.T.);
#3435=EDGE_CURVE('',#2892,#2894,#1990,.T.);
#3436=EDGE_CURVE('',#2895,#2893,#1991,.T.);
#3437=EDGE_CURVE('',#2895,#2896,#1992,.T.);
#3438=EDGE_CURVE('',#2894,#2896,#1993,.T.);
#3439=EDGE_CURVE('',#2897,#2895,#1994,.T.);
#3440=EDGE_CURVE('',#2898,#2897,#1995,.T.);
#3441=EDGE_CURVE('',#2896,#2898,#1996,.T.);
#3442=EDGE_CURVE('',#2899,#2899,#673,.T.);
#3443=EDGE_CURVE('',#2899,#2900,#1997,.T.);
#3444=EDGE_CURVE('',#2900,#2900,#674,.T.);
#3445=EDGE_CURVE('',#2837,#2901,#1998,.T.);
#3446=EDGE_CURVE('',#2901,#2902,#1999,.T.);
#3447=EDGE_CURVE('',#2838,#2902,#2000,.T.);
#3448=EDGE_CURVE('',#2903,#2822,#2001,.T.);
#3449=EDGE_CURVE('',#2904,#2903,#2002,.T.);
#3450=EDGE_CURVE('',#2904,#2820,#2003,.T.);
#3451=EDGE_CURVE('',#2857,#2904,#2004,.T.);
#3452=EDGE_CURVE('',#2858,#2903,#2005,.T.);
#3453=EDGE_CURVE('',#2905,#2842,#2006,.T.);
#3454=EDGE_CURVE('',#2906,#2905,#2007,.T.);
#3455=EDGE_CURVE('',#2906,#2840,#2008,.T.);
#3456=EDGE_CURVE('',#2877,#2906,#2009,.T.);
#3457=EDGE_CURVE('',#2878,#2905,#2010,.T.);
#3458=EDGE_CURVE('',#2907,#2862,#2011,.T.);
#3459=EDGE_CURVE('',#2908,#2907,#2012,.T.);
#3460=EDGE_CURVE('',#2908,#2860,#2013,.T.);
#3461=EDGE_CURVE('',#2897,#2908,#2014,.T.);
#3462=EDGE_CURVE('',#2898,#2907,#2015,.T.);
#3463=EDGE_CURVE('',#2902,#2882,#2016,.T.);
#3464=EDGE_CURVE('',#2901,#2880,#2017,.T.);
#3465=EDGE_CURVE('',#2909,#2909,#675,.T.);
#3466=EDGE_CURVE('',#2909,#2910,#2018,.T.);
#3467=EDGE_CURVE('',#2910,#2910,#676,.T.);
#3468=EDGE_CURVE('',#2911,#2911,#677,.T.);
#3469=EDGE_CURVE('',#2911,#2912,#2019,.T.);
#3470=EDGE_CURVE('',#2912,#2912,#678,.T.);
#3471=EDGE_CURVE('',#2913,#2913,#679,.T.);
#3472=EDGE_CURVE('',#2913,#2914,#2020,.T.);
#3473=EDGE_CURVE('',#2914,#2914,#680,.T.);
#3474=EDGE_CURVE('',#2915,#2915,#681,.T.);
#3475=EDGE_CURVE('',#2915,#2916,#2021,.T.);
#3476=EDGE_CURVE('',#2916,#2916,#682,.T.);
#3477=EDGE_CURVE('',#2917,#2917,#683,.T.);
#3478=EDGE_CURVE('',#2917,#2918,#2022,.T.);
#3479=EDGE_CURVE('',#2918,#2918,#684,.T.);
#3480=EDGE_CURVE('',#2919,#2919,#685,.T.);
#3481=EDGE_CURVE('',#2919,#2920,#2023,.T.);
#3482=EDGE_CURVE('',#2920,#2920,#686,.T.);
#3483=EDGE_CURVE('',#2921,#2921,#687,.T.);
#3484=EDGE_CURVE('',#2921,#2922,#2024,.T.);
#3485=EDGE_CURVE('',#2922,#2922,#688,.T.);
#3486=EDGE_CURVE('',#2923,#2923,#689,.T.);
#3487=EDGE_CURVE('',#2923,#2924,#2025,.T.);
#3488=EDGE_CURVE('',#2924,#2924,#690,.T.);
#3489=EDGE_CURVE('',#2925,#2925,#691,.T.);
#3490=EDGE_CURVE('',#2925,#2926,#2026,.T.);
#3491=EDGE_CURVE('',#2926,#2926,#692,.T.);
#3492=EDGE_CURVE('',#2927,#2927,#693,.T.);
#3493=EDGE_CURVE('',#2927,#2928,#2027,.T.);
#3494=EDGE_CURVE('',#2928,#2928,#694,.T.);
#3495=EDGE_CURVE('',#2929,#2929,#695,.T.);
#3496=EDGE_CURVE('',#2929,#2930,#2028,.T.);
#3497=EDGE_CURVE('',#2930,#2930,#696,.T.);
#3498=EDGE_CURVE('',#2931,#2931,#697,.T.);
#3499=EDGE_CURVE('',#2931,#2932,#2029,.T.);
#3500=EDGE_CURVE('',#2932,#2932,#698,.T.);
#3501=EDGE_CURVE('',#2933,#2934,#2030,.T.);
#3502=EDGE_CURVE('',#2934,#2935,#2031,.T.);
#3503=EDGE_CURVE('',#2936,#2935,#2032,.T.);
#3504=EDGE_CURVE('',#2933,#2936,#2033,.T.);
#3505=EDGE_CURVE('',#2937,#2933,#2034,.T.);
#3506=EDGE_CURVE('',#2938,#2936,#2035,.T.);
#3507=EDGE_CURVE('',#2937,#2938,#2036,.T.);
#3508=EDGE_CURVE('',#2939,#2937,#2037,.T.);
#3509=EDGE_CURVE('',#2940,#2938,#2038,.T.);
#3510=EDGE_CURVE('',#2939,#2940,#2039,.T.);
#3511=EDGE_CURVE('',#2934,#2939,#2040,.T.);
#3512=EDGE_CURVE('',#2935,#2940,#2041,.T.);
#3513=EDGE_CURVE('',#2941,#2942,#2042,.T.);
#3514=EDGE_CURVE('',#2943,#2941,#2043,.T.);
#3515=EDGE_CURVE('',#2944,#2943,#2044,.T.);
#3516=EDGE_CURVE('',#2942,#2944,#2045,.T.);
#3517=EDGE_CURVE('',#2943,#2945,#2046,.T.);
#3518=EDGE_CURVE('',#2946,#2945,#2047,.T.);
#3519=EDGE_CURVE('',#2944,#2946,#2048,.T.);
#3520=EDGE_CURVE('',#2945,#2947,#2049,.T.);
#3521=EDGE_CURVE('',#2947,#2948,#2050,.T.);
#3522=EDGE_CURVE('',#2948,#2946,#2051,.T.);
#3523=EDGE_CURVE('',#2949,#2949,#699,.T.);
#3524=EDGE_CURVE('',#2950,#2941,#2052,.T.);
#3525=EDGE_CURVE('',#2951,#2950,#2053,.T.);
#3526=EDGE_CURVE('',#2951,#2952,#2054,.T.);
#3527=EDGE_CURVE('',#2953,#2952,#2055,.T.);
#3528=EDGE_CURVE('',#2953,#2954,#2056,.T.);
#3529=EDGE_CURVE('',#2954,#2955,#2057,.T.);
#3530=EDGE_CURVE('',#2955,#2947,#2058,.T.);
#3531=EDGE_CURVE('',#2955,#2956,#2059,.T.);
#3532=EDGE_CURVE('',#2956,#2948,#2060,.T.);
#3533=EDGE_CURVE('',#2957,#2954,#2061,.T.);
#3534=EDGE_CURVE('',#2956,#2957,#2062,.T.);
#3535=EDGE_CURVE('',#2958,#2957,#2063,.T.);
#3536=EDGE_CURVE('',#2959,#2958,#2064,.T.);
#3537=EDGE_CURVE('',#2959,#2960,#2065,.T.);
#3538=EDGE_CURVE('',#2961,#2960,#2066,.T.);
#3539=EDGE_CURVE('',#2961,#2942,#2067,.T.);
#3540=EDGE_CURVE('',#2958,#2953,#2068,.T.);
#3541=EDGE_CURVE('',#2952,#2962,#2069,.T.);
#3542=EDGE_CURVE('',#2962,#2963,#375,.T.);
#3543=EDGE_CURVE('',#2963,#2959,#2070,.T.);
#3544=EDGE_CURVE('',#2964,#2962,#700,.F.);
#3545=EDGE_CURVE('',#2964,#2949,#2071,.T.);
#3546=EDGE_CURVE('',#2965,#2964,#701,.F.);
#3547=EDGE_CURVE('',#2966,#2965,#376,.T.);
#3548=EDGE_CURVE('',#2963,#2966,#702,.F.);
#3549=EDGE_CURVE('',#2965,#2951,#2072,.T.);
#3550=EDGE_CURVE('',#2960,#2966,#2073,.T.);
#3551=EDGE_CURVE('',#2950,#2961,#2074,.T.);
#3552=EDGE_CURVE('',#2967,#2967,#703,.T.);
#3553=EDGE_CURVE('',#2967,#2968,#2075,.T.);
#3554=EDGE_CURVE('',#2968,#2968,#704,.T.);
#3555=EDGE_CURVE('',#2968,#2969,#2076,.T.);
#3556=EDGE_CURVE('',#2969,#2969,#705,.T.);
#3557=EDGE_CURVE('',#2970,#2970,#706,.T.);
#3558=EDGE_CURVE('',#2970,#2971,#2077,.T.);
#3559=EDGE_CURVE('',#2971,#2971,#707,.T.);
#3560=EDGE_CURVE('',#2972,#2973,#2078,.T.);
#3561=EDGE_CURVE('',#2973,#2974,#2079,.T.);
#3562=EDGE_CURVE('',#2975,#2974,#2080,.T.);
#3563=EDGE_CURVE('',#2972,#2975,#2081,.T.);
#3564=EDGE_CURVE('',#2976,#2972,#2082,.T.);
#3565=EDGE_CURVE('',#2977,#2975,#2083,.T.);
#3566=EDGE_CURVE('',#2976,#2977,#2084,.T.);
#3567=EDGE_CURVE('',#2978,#2976,#2085,.T.);
#3568=EDGE_CURVE('',#2979,#2977,#2086,.T.);
#3569=EDGE_CURVE('',#2978,#2979,#2087,.T.);
#3570=EDGE_CURVE('',#2973,#2978,#2088,.T.);
#3571=EDGE_CURVE('',#2974,#2979,#2089,.T.);
#3572=EDGE_CURVE('',#2980,#2981,#2090,.T.);
#3573=EDGE_CURVE('',#2981,#2982,#2091,.T.);
#3574=EDGE_CURVE('',#2983,#2982,#2092,.T.);
#3575=EDGE_CURVE('',#2980,#2983,#2093,.T.);
#3576=EDGE_CURVE('',#2984,#2980,#2094,.T.);
#3577=EDGE_CURVE('',#2985,#2983,#2095,.T.);
#3578=EDGE_CURVE('',#2984,#2985,#2096,.T.);
#3579=EDGE_CURVE('',#2986,#2984,#2097,.T.);
#3580=EDGE_CURVE('',#2987,#2985,#2098,.T.);
#3581=EDGE_CURVE('',#2986,#2987,#2099,.T.);
#3582=EDGE_CURVE('',#2981,#2986,#2100,.T.);
#3583=EDGE_CURVE('',#2982,#2987,#2101,.T.);
#3584=EDGE_CURVE('',#2988,#2988,#708,.T.);
#3585=EDGE_CURVE('',#2988,#2989,#2102,.T.);
#3586=EDGE_CURVE('',#2989,#2989,#709,.T.);
#3587=EDGE_CURVE('',#2990,#2990,#710,.T.);
#3588=EDGE_CURVE('',#2990,#2991,#2103,.T.);
#3589=EDGE_CURVE('',#2991,#2991,#711,.T.);
#3590=EDGE_CURVE('',#2992,#2993,#712,.T.);
#3591=EDGE_CURVE('',#2994,#2992,#2104,.T.);
#3592=EDGE_CURVE('',#2995,#2994,#713,.T.);
#3593=EDGE_CURVE('',#2993,#2995,#2105,.T.);
#3594=EDGE_CURVE('',#2996,#2994,#2106,.T.);
#3595=EDGE_CURVE('',#2997,#2996,#2107,.T.);
#3596=EDGE_CURVE('',#2997,#2998,#2108,.T.);
#3597=EDGE_CURVE('',#2998,#2999,#2109,.T.);
#3598=EDGE_CURVE('',#2995,#2999,#2110,.T.);
#3599=EDGE_CURVE('',#3000,#3000,#714,.T.);
#3600=EDGE_CURVE('',#3001,#3001,#715,.T.);
#3601=EDGE_CURVE('',#2992,#3002,#2111,.T.);
#3602=EDGE_CURVE('',#3002,#2996,#2112,.T.);
#3603=EDGE_CURVE('',#3003,#3003,#716,.T.);
#3604=EDGE_CURVE('',#3003,#3001,#2113,.T.);
#3605=EDGE_CURVE('',#3004,#3004,#717,.T.);
#3606=EDGE_CURVE('',#3004,#3000,#2114,.T.);
#3607=EDGE_CURVE('',#3005,#3006,#2115,.T.);
#3608=EDGE_CURVE('',#3005,#3007,#2116,.T.);
#3609=EDGE_CURVE('',#3008,#3007,#2117,.T.);
#3610=EDGE_CURVE('',#3006,#3008,#2118,.T.);
#3611=EDGE_CURVE('',#3006,#3009,#2119,.T.);
#3612=EDGE_CURVE('',#3009,#3010,#2120,.T.);
#3613=EDGE_CURVE('',#3010,#3005,#2121,.T.);
#3614=EDGE_CURVE('',#3010,#2997,#2122,.T.);
#3615=EDGE_CURVE('',#3007,#3002,#2123,.T.);
#3616=EDGE_CURVE('',#3011,#2993,#2124,.T.);
#3617=EDGE_CURVE('',#3008,#3011,#2125,.T.);
#3618=EDGE_CURVE('',#2998,#3009,#2126,.T.);
#3619=EDGE_CURVE('',#2999,#3011,#2127,.T.);
#3620=EDGE_CURVE('',#3012,#3012,#718,.T.);
#3621=EDGE_CURVE('',#3012,#3013,#2128,.T.);
#3622=EDGE_CURVE('',#3013,#3013,#719,.T.);
#3623=EDGE_CURVE('',#3014,#3014,#720,.T.);
#3624=EDGE_CURVE('',#3015,#3015,#721,.T.);
#3625=EDGE_CURVE('',#3014,#3016,#2129,.T.);
#3626=EDGE_CURVE('',#3016,#3016,#722,.T.);
#3627=EDGE_CURVE('',#3017,#3017,#723,.T.);
#3628=EDGE_CURVE('',#3017,#3015,#2130,.T.);
#3629=EDGE_CURVE('',#3018,#3018,#724,.T.);
#3630=EDGE_CURVE('',#3018,#3019,#2131,.T.);
#3631=EDGE_CURVE('',#3019,#3019,#725,.T.);
#3632=EDGE_CURVE('',#3020,#3020,#726,.T.);
#3633=EDGE_CURVE('',#3020,#3021,#2132,.T.);
#3634=EDGE_CURVE('',#3021,#3021,#727,.T.);
#3635=EDGE_CURVE('',#3022,#3022,#728,.T.);
#3636=EDGE_CURVE('',#3022,#3023,#2133,.T.);
#3637=EDGE_CURVE('',#3023,#3023,#729,.T.);
#3638=EDGE_CURVE('',#3024,#3024,#730,.T.);
#3639=EDGE_CURVE('',#3024,#3025,#2134,.T.);
#3640=EDGE_CURVE('',#3025,#3025,#731,.T.);
#3641=EDGE_CURVE('',#3026,#3026,#732,.T.);
#3642=EDGE_CURVE('',#3026,#3027,#2135,.T.);
#3643=EDGE_CURVE('',#3027,#3027,#733,.T.);
#3644=EDGE_CURVE('',#3028,#3028,#734,.T.);
#3645=EDGE_CURVE('',#3028,#3029,#2136,.T.);
#3646=EDGE_CURVE('',#3029,#3029,#735,.T.);
#3647=EDGE_CURVE('',#3030,#3030,#736,.T.);
#3648=EDGE_CURVE('',#3030,#3031,#2137,.T.);
#3649=EDGE_CURVE('',#3031,#3031,#737,.T.);
#3650=EDGE_CURVE('',#3032,#3032,#738,.T.);
#3651=EDGE_CURVE('',#3033,#3033,#739,.T.);
#3652=EDGE_CURVE('',#3032,#3034,#2138,.T.);
#3653=EDGE_CURVE('',#3034,#3034,#740,.T.);
#3654=EDGE_CURVE('',#3035,#3035,#741,.T.);
#3655=EDGE_CURVE('',#3035,#3033,#2139,.T.);
#3656=EDGE_CURVE('',#3036,#3036,#742,.T.);
#3657=EDGE_CURVE('',#3036,#3037,#2140,.T.);
#3658=EDGE_CURVE('',#3037,#3037,#743,.T.);
#3659=EDGE_CURVE('',#3038,#3038,#744,.T.);
#3660=EDGE_CURVE('',#3038,#3039,#2141,.T.);
#3661=EDGE_CURVE('',#3039,#3039,#745,.T.);
#3662=EDGE_CURVE('',#3040,#3040,#746,.T.);
#3663=EDGE_CURVE('',#3040,#3041,#2142,.T.);
#3664=EDGE_CURVE('',#3041,#3041,#747,.T.);
#3665=EDGE_CURVE('',#3042,#3042,#748,.T.);
#3666=EDGE_CURVE('',#3042,#3043,#2143,.T.);
#3667=EDGE_CURVE('',#3043,#3043,#749,.T.);
#3668=EDGE_CURVE('',#3044,#3044,#750,.T.);
#3669=EDGE_CURVE('',#3044,#3045,#2144,.T.);
#3670=EDGE_CURVE('',#3045,#3045,#751,.T.);
#3671=EDGE_CURVE('',#3046,#3046,#752,.T.);
#3672=EDGE_CURVE('',#3046,#3047,#2145,.T.);
#3673=EDGE_CURVE('',#3047,#3047,#753,.T.);
#3674=EDGE_CURVE('',#3048,#3049,#754,.T.);
#3675=EDGE_CURVE('',#3050,#3048,#2146,.T.);
#3676=EDGE_CURVE('',#3051,#3050,#755,.T.);
#3677=EDGE_CURVE('',#3049,#3051,#2147,.T.);
#3678=EDGE_CURVE('',#3052,#3050,#2148,.T.);
#3679=EDGE_CURVE('',#3053,#3052,#2149,.T.);
#3680=EDGE_CURVE('',#3053,#3054,#2150,.T.);
#3681=EDGE_CURVE('',#3054,#3055,#2151,.T.);
#3682=EDGE_CURVE('',#3051,#3055,#2152,.T.);
#3683=EDGE_CURVE('',#3056,#3056,#756,.T.);
#3684=EDGE_CURVE('',#3057,#3057,#757,.T.);
#3685=EDGE_CURVE('',#3048,#3058,#2153,.T.);
#3686=EDGE_CURVE('',#3058,#3052,#2154,.T.);
#3687=EDGE_CURVE('',#3059,#3059,#758,.T.);
#3688=EDGE_CURVE('',#3059,#3057,#2155,.T.);
#3689=EDGE_CURVE('',#3060,#3060,#759,.T.);
#3690=EDGE_CURVE('',#3060,#3056,#2156,.T.);
#3691=EDGE_CURVE('',#3061,#3062,#2157,.T.);
#3692=EDGE_CURVE('',#3061,#3063,#2158,.T.);
#3693=EDGE_CURVE('',#3064,#3063,#2159,.T.);
#3694=EDGE_CURVE('',#3062,#3064,#2160,.T.);
#3695=EDGE_CURVE('',#3062,#3065,#2161,.T.);
#3696=EDGE_CURVE('',#3065,#3066,#2162,.T.);
#3697=EDGE_CURVE('',#3066,#3061,#2163,.T.);
#3698=EDGE_CURVE('',#3066,#3053,#2164,.T.);
#3699=EDGE_CURVE('',#3063,#3058,#2165,.T.);
#3700=EDGE_CURVE('',#3067,#3049,#2166,.T.);
#3701=EDGE_CURVE('',#3064,#3067,#2167,.T.);
#3702=EDGE_CURVE('',#3054,#3065,#2168,.T.);
#3703=EDGE_CURVE('',#3055,#3067,#2169,.T.);
#3704=EDGE_CURVE('',#3068,#3069,#2170,.T.);
#3705=EDGE_CURVE('',#3069,#3070,#2171,.T.);
#3706=EDGE_CURVE('',#3070,#3071,#2172,.T.);
#3707=EDGE_CURVE('',#3068,#3071,#2173,.T.);
#3708=EDGE_CURVE('',#3069,#3072,#2174,.T.);
#3709=EDGE_CURVE('',#3072,#3073,#2175,.T.);
#3710=EDGE_CURVE('',#3073,#3070,#2176,.T.);
#3711=EDGE_CURVE('',#3072,#3074,#2177,.T.);
#3712=EDGE_CURVE('',#3074,#3075,#2178,.T.);
#3713=EDGE_CURVE('',#3075,#3073,#2179,.T.);
#3714=EDGE_CURVE('',#3074,#3076,#2180,.T.);
#3715=EDGE_CURVE('',#3076,#3077,#2181,.T.);
#3716=EDGE_CURVE('',#3077,#3075,#2182,.T.);
#3717=EDGE_CURVE('',#3076,#3078,#2183,.T.);
#3718=EDGE_CURVE('',#3078,#3079,#2184,.T.);
#3719=EDGE_CURVE('',#3079,#3077,#2185,.T.);
#3720=EDGE_CURVE('',#3078,#3068,#2186,.T.);
#3721=EDGE_CURVE('',#3071,#3079,#2187,.T.);
#3722=EDGE_CURVE('',#3080,#3080,#760,.T.);
#3723=EDGE_CURVE('',#3081,#3081,#761,.T.);
#3724=EDGE_CURVE('',#3082,#3082,#762,.T.);
#3725=EDGE_CURVE('',#3082,#3081,#2188,.T.);
#3726=EDGE_CURVE('',#3083,#3083,#763,.T.);
#3727=EDGE_CURVE('',#3083,#3082,#2189,.T.);
#3728=EDGE_CURVE('',#3084,#3084,#764,.T.);
#3729=EDGE_CURVE('',#3084,#3083,#2190,.T.);
#3730=EDGE_CURVE('',#3085,#3085,#765,.T.);
#3731=EDGE_CURVE('',#3086,#3086,#766,.F.);
#3732=EDGE_CURVE('',#3086,#3085,#2191,.T.);
#3733=EDGE_CURVE('',#3080,#3086,#2192,.T.);
#3734=EDGE_CURVE('',#3087,#3087,#767,.T.);
#3735=EDGE_CURVE('',#3087,#3088,#2193,.T.);
#3736=EDGE_CURVE('',#3088,#3088,#768,.T.);
#3737=EDGE_CURVE('',#3089,#3089,#769,.T.);
#3738=EDGE_CURVE('',#3090,#3090,#770,.T.);
#3739=EDGE_CURVE('',#3089,#3091,#2194,.T.);
#3740=EDGE_CURVE('',#3091,#3091,#771,.T.);
#3741=EDGE_CURVE('',#3092,#3092,#772,.T.);
#3742=EDGE_CURVE('',#3092,#3090,#2195,.T.);
#3743=EDGE_CURVE('',#3093,#3093,#773,.T.);
#3744=EDGE_CURVE('',#3093,#3094,#2196,.T.);
#3745=EDGE_CURVE('',#3094,#3094,#774,.T.);
#3746=EDGE_CURVE('',#3095,#3095,#775,.T.);
#3747=EDGE_CURVE('',#3095,#3096,#2197,.T.);
#3748=EDGE_CURVE('',#3096,#3096,#776,.T.);
#3749=EDGE_CURVE('',#3097,#3097,#777,.T.);
#3750=EDGE_CURVE('',#3097,#3098,#2198,.T.);
#3751=EDGE_CURVE('',#3098,#3098,#778,.T.);
#3752=EDGE_CURVE('',#3099,#3099,#779,.T.);
#3753=EDGE_CURVE('',#3099,#3100,#2199,.T.);
#3754=EDGE_CURVE('',#3100,#3100,#780,.T.);
#3755=EDGE_CURVE('',#3101,#3101,#781,.T.);
#3756=EDGE_CURVE('',#3101,#3102,#2200,.T.);
#3757=EDGE_CURVE('',#3102,#3102,#782,.T.);
#3758=EDGE_CURVE('',#3103,#3103,#783,.T.);
#3759=EDGE_CURVE('',#3104,#3104,#784,.T.);
#3760=EDGE_CURVE('',#3103,#3105,#2201,.T.);
#3761=EDGE_CURVE('',#3105,#3105,#785,.T.);
#3762=EDGE_CURVE('',#3106,#3106,#786,.T.);
#3763=EDGE_CURVE('',#3106,#3104,#2202,.T.);
#3764=EDGE_CURVE('',#3107,#3107,#787,.T.);
#3765=EDGE_CURVE('',#3107,#3108,#2203,.T.);
#3766=EDGE_CURVE('',#3108,#3108,#788,.T.);
#3767=EDGE_CURVE('',#3109,#3109,#789,.T.);
#3768=EDGE_CURVE('',#3109,#3110,#2204,.T.);
#3769=EDGE_CURVE('',#3110,#3110,#790,.T.);
#3770=EDGE_CURVE('',#3111,#3111,#791,.T.);
#3771=EDGE_CURVE('',#3111,#3112,#2205,.T.);
#3772=EDGE_CURVE('',#3112,#3112,#792,.T.);
#3773=EDGE_CURVE('',#3113,#3113,#793,.T.);
#3774=EDGE_CURVE('',#3113,#3114,#2206,.T.);
#3775=EDGE_CURVE('',#3114,#3114,#794,.T.);
#3776=EDGE_CURVE('',#3115,#3116,#2207,.T.);
#3777=EDGE_CURVE('',#3116,#3117,#2208,.T.);
#3778=EDGE_CURVE('',#3117,#3118,#2209,.T.);
#3779=EDGE_CURVE('',#3115,#3118,#2210,.T.);
#3780=EDGE_CURVE('',#3116,#3119,#2211,.T.);
#3781=EDGE_CURVE('',#3119,#3120,#2212,.T.);
#3782=EDGE_CURVE('',#3120,#3117,#2213,.T.);
#3783=EDGE_CURVE('',#3119,#3121,#2214,.T.);
#3784=EDGE_CURVE('',#3121,#3122,#2215,.T.);
#3785=EDGE_CURVE('',#3122,#3120,#2216,.T.);
#3786=EDGE_CURVE('',#3121,#3123,#2217,.T.);
#3787=EDGE_CURVE('',#3123,#3124,#2218,.T.);
#3788=EDGE_CURVE('',#3124,#3122,#2219,.T.);
#3789=EDGE_CURVE('',#3123,#3125,#2220,.T.);
#3790=EDGE_CURVE('',#3125,#3126,#2221,.T.);
#3791=EDGE_CURVE('',#3126,#3124,#2222,.T.);
#3792=EDGE_CURVE('',#3125,#3115,#2223,.T.);
#3793=EDGE_CURVE('',#3118,#3126,#2224,.T.);
#3794=EDGE_CURVE('',#3127,#3127,#795,.T.);
#3795=EDGE_CURVE('',#3128,#3128,#796,.T.);
#3796=EDGE_CURVE('',#3129,#3129,#797,.T.);
#3797=EDGE_CURVE('',#3129,#3128,#2225,.T.);
#3798=EDGE_CURVE('',#3130,#3130,#798,.T.);
#3799=EDGE_CURVE('',#3130,#3129,#2226,.T.);
#3800=EDGE_CURVE('',#3131,#3131,#799,.T.);
#3801=EDGE_CURVE('',#3131,#3130,#2227,.T.);
#3802=EDGE_CURVE('',#3132,#3132,#800,.T.);
#3803=EDGE_CURVE('',#3133,#3133,#801,.F.);
#3804=EDGE_CURVE('',#3133,#3132,#2228,.T.);
#3805=EDGE_CURVE('',#3127,#3133,#2229,.T.);
#3806=EDGE_CURVE('',#3134,#3134,#802,.T.);
#3807=EDGE_CURVE('',#3134,#3135,#2230,.T.);
#3808=EDGE_CURVE('',#3135,#3135,#803,.T.);
#3809=EDGE_CURVE('',#3136,#3136,#804,.T.);
#3810=EDGE_CURVE('',#3136,#3137,#2231,.T.);
#3811=EDGE_CURVE('',#3137,#3137,#805,.T.);
#3812=EDGE_CURVE('',#3138,#3138,#806,.T.);
#3813=EDGE_CURVE('',#3138,#3139,#2232,.T.);
#3814=EDGE_CURVE('',#3139,#3139,#807,.T.);
#3815=EDGE_CURVE('',#3140,#3141,#2233,.T.);
#3816=EDGE_CURVE('',#3141,#3142,#2234,.T.);
#3817=EDGE_CURVE('',#3143,#3142,#2235,.T.);
#3818=EDGE_CURVE('',#3140,#3143,#2236,.T.);
#3819=EDGE_CURVE('',#3144,#3140,#2237,.T.);
#3820=EDGE_CURVE('',#3145,#3143,#2238,.T.);
#3821=EDGE_CURVE('',#3144,#3145,#2239,.T.);
#3822=EDGE_CURVE('',#3146,#3144,#2240,.T.);
#3823=EDGE_CURVE('',#3147,#3145,#2241,.T.);
#3824=EDGE_CURVE('',#3146,#3147,#2242,.T.);
#3825=EDGE_CURVE('',#3141,#3146,#2243,.T.);
#3826=EDGE_CURVE('',#3142,#3147,#2244,.T.);
#3827=EDGE_CURVE('',#3148,#3149,#2245,.T.);
#3828=EDGE_CURVE('',#3149,#3150,#2246,.T.);
#3829=EDGE_CURVE('',#3150,#3151,#2247,.T.);
#3830=EDGE_CURVE('',#3148,#3151,#2248,.T.);
#3831=EDGE_CURVE('',#3149,#3152,#2249,.T.);
#3832=EDGE_CURVE('',#3152,#3153,#2250,.T.);
#3833=EDGE_CURVE('',#3153,#3150,#2251,.T.);
#3834=EDGE_CURVE('',#3152,#3154,#2252,.T.);
#3835=EDGE_CURVE('',#3154,#3155,#2253,.T.);
#3836=EDGE_CURVE('',#3155,#3153,#2254,.T.);
#3837=EDGE_CURVE('',#3154,#3156,#2255,.T.);
#3838=EDGE_CURVE('',#3156,#3157,#2256,.T.);
#3839=EDGE_CURVE('',#3157,#3155,#2257,.T.);
#3840=EDGE_CURVE('',#3156,#3158,#2258,.T.);
#3841=EDGE_CURVE('',#3158,#3159,#2259,.T.);
#3842=EDGE_CURVE('',#3159,#3157,#2260,.T.);
#3843=EDGE_CURVE('',#3158,#3148,#2261,.T.);
#3844=EDGE_CURVE('',#3151,#3159,#2262,.T.);
#3845=EDGE_CURVE('',#3160,#3160,#808,.T.);
#3846=EDGE_CURVE('',#3161,#3161,#809,.T.);
#3847=EDGE_CURVE('',#3162,#3162,#810,.T.);
#3848=EDGE_CURVE('',#3162,#3161,#2263,.T.);
#3849=EDGE_CURVE('',#3163,#3163,#811,.T.);
#3850=EDGE_CURVE('',#3163,#3162,#2264,.T.);
#3851=EDGE_CURVE('',#3164,#3164,#812,.T.);
#3852=EDGE_CURVE('',#3164,#3163,#2265,.T.);
#3853=EDGE_CURVE('',#3165,#3165,#813,.T.);
#3854=EDGE_CURVE('',#3166,#3166,#814,.F.);
#3855=EDGE_CURVE('',#3166,#3165,#2266,.T.);
#3856=EDGE_CURVE('',#3160,#3166,#2267,.T.);
#3857=EDGE_CURVE('',#3167,#3168,#2268,.T.);
#3858=EDGE_CURVE('',#3167,#3169,#815,.T.);
#3859=EDGE_CURVE('',#3169,#3168,#816,.T.);
#3860=EDGE_CURVE('',#3170,#3167,#329,.T.);
#3861=EDGE_CURVE('',#3171,#3170,#817,.T.);
#3862=EDGE_CURVE('',#3168,#3171,#330,.T.);
#3863=EDGE_CURVE('',#3169,#3172,#2269,.T.);
#3864=EDGE_CURVE('',#3172,#3172,#818,.T.);
#3865=EDGE_CURVE('',#3171,#3170,#2270,.T.);
#3866=EDGE_CURVE('',#3173,#3174,#2271,.T.);
#3867=EDGE_CURVE('',#3173,#3175,#819,.T.);
#3868=EDGE_CURVE('',#3175,#3174,#820,.T.);
#3869=EDGE_CURVE('',#3176,#3173,#331,.T.);
#3870=EDGE_CURVE('',#3177,#3176,#821,.T.);
#3871=EDGE_CURVE('',#3174,#3177,#332,.T.);
#3872=EDGE_CURVE('',#3175,#3178,#2272,.T.);
#3873=EDGE_CURVE('',#3178,#3178,#822,.T.);
#3874=EDGE_CURVE('',#3177,#3176,#2273,.T.);
#3875=EDGE_CURVE('',#3179,#3179,#823,.T.);
#3876=EDGE_CURVE('',#3179,#3180,#2274,.T.);
#3877=EDGE_CURVE('',#3180,#3180,#824,.T.);
#3878=EDGE_CURVE('',#3181,#3181,#825,.T.);
#3879=EDGE_CURVE('',#3181,#3182,#2275,.T.);
#3880=EDGE_CURVE('',#3182,#3182,#826,.T.);
#3881=EDGE_CURVE('',#3183,#3184,#2276,.T.);
#3882=EDGE_CURVE('',#3184,#3185,#2277,.T.);
#3883=EDGE_CURVE('',#3186,#3185,#2278,.T.);
#3884=EDGE_CURVE('',#3183,#3186,#2279,.T.);
#3885=EDGE_CURVE('',#3187,#3183,#2280,.T.);
#3886=EDGE_CURVE('',#3188,#3186,#2281,.T.);
#3887=EDGE_CURVE('',#3187,#3188,#2282,.T.);
#3888=EDGE_CURVE('',#3189,#3187,#2283,.T.);
#3889=EDGE_CURVE('',#3190,#3188,#2284,.T.);
#3890=EDGE_CURVE('',#3189,#3190,#2285,.T.);
#3891=EDGE_CURVE('',#3184,#3189,#2286,.T.);
#3892=EDGE_CURVE('',#3185,#3190,#2287,.T.);
#3893=EDGE_CURVE('',#3191,#3192,#2288,.T.);
#3894=EDGE_CURVE('',#3191,#3193,#2289,.T.);
#3895=EDGE_CURVE('',#3193,#3194,#2290,.T.);
#3896=EDGE_CURVE('',#3192,#3194,#2291,.T.);
#3897=EDGE_CURVE('',#3195,#3191,#2292,.T.);
#3898=EDGE_CURVE('',#3195,#3196,#2293,.T.);
#3899=EDGE_CURVE('',#3196,#3193,#2294,.T.);
#3900=EDGE_CURVE('',#3197,#3195,#2295,.T.);
#3901=EDGE_CURVE('',#3197,#3198,#2296,.T.);
#3902=EDGE_CURVE('',#3198,#3196,#2297,.T.);
#3903=EDGE_CURVE('',#3199,#3197,#2298,.T.);
#3904=EDGE_CURVE('',#3199,#3200,#2299,.T.);
#3905=EDGE_CURVE('',#3200,#3198,#2300,.T.);
#3906=EDGE_CURVE('',#3201,#3199,#2301,.T.);
#3907=EDGE_CURVE('',#3201,#3202,#2302,.T.);
#3908=EDGE_CURVE('',#3202,#3200,#2303,.T.);
#3909=EDGE_CURVE('',#3192,#3201,#2304,.T.);
#3910=EDGE_CURVE('',#3194,#3202,#2305,.T.);
#3911=EDGE_CURVE('',#3203,#3203,#827,.T.);
#3912=EDGE_CURVE('',#3204,#3204,#828,.T.);
#3913=EDGE_CURVE('',#3204,#3203,#2306,.T.);
#3914=EDGE_CURVE('',#3205,#3205,#829,.F.);
#3915=EDGE_CURVE('',#3205,#3204,#2307,.T.);
#3916=EDGE_CURVE('',#3206,#3206,#830,.T.);
#3917=EDGE_CURVE('',#3206,#3205,#2308,.T.);
#3918=EDGE_CURVE('',#3207,#3207,#831,.T.);
#3919=EDGE_CURVE('',#3207,#3208,#2309,.T.);
#3920=EDGE_CURVE('',#3208,#3208,#832,.T.);
#3921=EDGE_CURVE('',#3209,#3210,#333,.T.);
#3922=EDGE_CURVE('',#3210,#3209,#334,.T.);
#3923=EDGE_CURVE('',#3210,#3211,#2310,.T.);
#3924=EDGE_CURVE('',#3211,#3211,#833,.T.);
#3925=EDGE_CURVE('',#3212,#3212,#834,.T.);
#3926=EDGE_CURVE('',#3212,#3213,#2311,.T.);
#3927=EDGE_CURVE('',#3213,#3213,#835,.T.);
#3928=EDGE_CURVE('',#3214,#3214,#836,.T.);
#3929=EDGE_CURVE('',#3214,#3215,#2312,.T.);
#3930=EDGE_CURVE('',#3215,#3215,#837,.T.);
#3931=EDGE_CURVE('',#3216,#3217,#2313,.T.);
#3932=EDGE_CURVE('',#3216,#3218,#2314,.T.);
#3933=EDGE_CURVE('',#3219,#3218,#2315,.T.);
#3934=EDGE_CURVE('',#3217,#3219,#2316,.T.);
#3935=EDGE_CURVE('',#3217,#3220,#2317,.T.);
#3936=EDGE_CURVE('',#3221,#3219,#2318,.T.);
#3937=EDGE_CURVE('',#3220,#3221,#2319,.T.);
#3938=EDGE_CURVE('',#3220,#3216,#2320,.T.);
#3939=EDGE_CURVE('',#3218,#3221,#2321,.T.);
#3940=EDGE_CURVE('',#3222,#3222,#838,.T.);
#3941=EDGE_CURVE('',#3222,#3223,#2322,.T.);
#3942=EDGE_CURVE('',#3223,#3223,#839,.T.);
#3943=EDGE_CURVE('',#3224,#3224,#840,.T.);
#3944=EDGE_CURVE('',#3224,#3225,#2323,.T.);
#3945=EDGE_CURVE('',#3225,#3225,#841,.T.);
#3946=EDGE_CURVE('',#3226,#3226,#842,.T.);
#3947=EDGE_CURVE('',#3226,#3227,#2324,.T.);
#3948=EDGE_CURVE('',#3227,#3227,#843,.T.);
#3949=EDGE_CURVE('',#3228,#3228,#844,.T.);
#3950=EDGE_CURVE('',#3228,#3229,#2325,.T.);
#3951=EDGE_CURVE('',#3229,#3229,#845,.T.);
#3952=EDGE_CURVE('',#3230,#3230,#846,.T.);
#3953=EDGE_CURVE('',#3230,#3231,#2326,.T.);
#3954=EDGE_CURVE('',#3231,#3231,#847,.T.);
#3955=EDGE_CURVE('',#3232,#3232,#848,.T.);
#3956=EDGE_CURVE('',#3232,#3233,#2327,.T.);
#3957=EDGE_CURVE('',#3233,#3233,#849,.T.);
#3958=EDGE_CURVE('',#3234,#3234,#850,.T.);
#3959=EDGE_CURVE('',#3234,#3235,#2328,.T.);
#3960=EDGE_CURVE('',#3235,#3235,#851,.T.);
#3961=EDGE_CURVE('',#3236,#3236,#852,.T.);
#3962=EDGE_CURVE('',#3236,#3237,#2329,.T.);
#3963=EDGE_CURVE('',#3237,#3237,#853,.T.);
#3964=EDGE_CURVE('',#3238,#3239,#854,.T.);
#3965=EDGE_CURVE('',#3239,#3238,#855,.T.);
#3966=EDGE_CURVE('',#3239,#3240,#856,.T.);
#3967=EDGE_CURVE('',#3241,#3240,#857,.T.);
#3968=EDGE_CURVE('',#3240,#3241,#858,.T.);
#3969=EDGE_CURVE('',#3241,#3242,#2330,.T.);
#3970=EDGE_CURVE('',#3242,#3242,#859,.T.);
#3971=EDGE_CURVE('',#3243,#3243,#860,.T.);
#3972=EDGE_CURVE('',#3243,#3244,#2331,.T.);
#3973=EDGE_CURVE('',#3244,#3244,#861,.T.);
#3974=EDGE_CURVE('',#3244,#3245,#2332,.T.);
#3975=EDGE_CURVE('',#3245,#3245,#862,.T.);
#3976=EDGE_CURVE('',#3246,#3246,#863,.T.);
#3977=EDGE_CURVE('',#3246,#3238,#2333,.T.);
#3978=EDGE_CURVE('',#3247,#3247,#864,.T.);
#3979=EDGE_CURVE('',#3247,#3243,#2334,.T.);
#3980=EDGE_CURVE('',#3248,#3249,#865,.T.);
#3981=EDGE_CURVE('',#3249,#3248,#866,.T.);
#3982=EDGE_CURVE('',#3249,#3250,#867,.T.);
#3983=EDGE_CURVE('',#3251,#3250,#868,.T.);
#3984=EDGE_CURVE('',#3250,#3251,#869,.T.);
#3985=EDGE_CURVE('',#3252,#3252,#870,.T.);
#3986=EDGE_CURVE('',#3252,#3251,#2335,.T.);
#3987=EDGE_CURVE('',#3253,#3253,#871,.T.);
#3988=EDGE_CURVE('',#3254,#3254,#872,.T.);
#3989=EDGE_CURVE('',#3255,#3255,#873,.T.);
#3990=EDGE_CURVE('',#3255,#3253,#2336,.T.);
#3991=EDGE_CURVE('',#3256,#3256,#874,.T.);
#3992=EDGE_CURVE('',#3256,#3255,#2337,.T.);
#3993=EDGE_CURVE('',#3257,#3257,#875,.T.);
#3994=EDGE_CURVE('',#3257,#3256,#2338,.T.);
#3995=EDGE_CURVE('',#3248,#3254,#2339,.T.);
#3996=EDGE_CURVE('',#3258,#3259,#876,.T.);
#3997=EDGE_CURVE('',#3260,#3261,#877,.T.);
#3998=EDGE_CURVE('',#3262,#3263,#878,.T.);
#3999=EDGE_CURVE('',#3264,#3265,#879,.T.);
#4000=EDGE_CURVE('',#3266,#3267,#880,.T.);
#4001=EDGE_CURVE('',#3268,#3269,#881,.T.);
#4002=EDGE_CURVE('',#3270,#3271,#882,.T.);
#4003=EDGE_CURVE('',#3272,#3273,#883,.T.);
#4004=EDGE_CURVE('',#3274,#3275,#335,.T.);
#4005=EDGE_CURVE('',#3276,#3274,#884,.T.);
#4006=EDGE_CURVE('',#3277,#3276,#336,.T.);
#4007=EDGE_CURVE('',#3275,#3277,#885,.T.);
#4008=EDGE_CURVE('',#3278,#3276,#886,.T.);
#4009=EDGE_CURVE('',#3278,#3279,#337,.T.);
#4010=EDGE_CURVE('',#3280,#3279,#887,.T.);
#4011=EDGE_CURVE('',#3280,#3281,#338,.T.);
#4012=EDGE_CURVE('',#3282,#3281,#888,.T.);
#4013=EDGE_CURVE('',#3282,#3283,#339,.T.);
#4014=EDGE_CURVE('',#3283,#3284,#2340,.T.);
#4015=EDGE_CURVE('',#3284,#3284,#889,.T.);
#4016=EDGE_CURVE('',#3283,#3285,#340,.T.);
#4017=EDGE_CURVE('',#3286,#3285,#890,.T.);
#4018=EDGE_CURVE('',#3286,#3287,#341,.T.);
#4019=EDGE_CURVE('',#3288,#3287,#891,.T.);
#4020=EDGE_CURVE('',#3288,#3289,#342,.T.);
#4021=EDGE_CURVE('',#3290,#3289,#892,.T.);
#4022=EDGE_CURVE('',#3290,#3291,#343,.T.);
#4023=EDGE_CURVE('',#3292,#3291,#893,.T.);
#4024=EDGE_CURVE('',#3292,#3293,#344,.T.);
#4025=EDGE_CURVE('',#3277,#3293,#894,.T.);
#4026=EDGE_CURVE('',#3274,#3294,#895,.T.);
#4027=EDGE_CURVE('',#3294,#3278,#896,.T.);
#4028=EDGE_CURVE('',#3295,#3294,#345,.T.);
#4029=EDGE_CURVE('',#3279,#3295,#897,.T.);
#4030=EDGE_CURVE('',#3295,#3296,#898,.T.);
#4031=EDGE_CURVE('',#3296,#3280,#899,.T.);
#4032=EDGE_CURVE('',#3297,#3296,#346,.T.);
#4033=EDGE_CURVE('',#3281,#3297,#900,.T.);
#4034=EDGE_CURVE('',#3297,#3298,#901,.T.);
#4035=EDGE_CURVE('',#3298,#3282,#902,.T.);
#4036=EDGE_CURVE('',#3299,#3300,#347,.T.);
#4037=EDGE_CURVE('',#3285,#3299,#903,.T.);
#4038=EDGE_CURVE('',#3300,#3298,#348,.T.);
#4039=EDGE_CURVE('',#3299,#3301,#904,.T.);
#4040=EDGE_CURVE('',#3301,#3286,#905,.T.);
#4041=EDGE_CURVE('',#3302,#3301,#349,.T.);
#4042=EDGE_CURVE('',#3287,#3302,#906,.T.);
#4043=EDGE_CURVE('',#3302,#3303,#907,.T.);
#4044=EDGE_CURVE('',#3303,#3288,#908,.T.);
#4045=EDGE_CURVE('',#3304,#3303,#350,.T.);
#4046=EDGE_CURVE('',#3289,#3304,#909,.T.);
#4047=EDGE_CURVE('',#3304,#3305,#910,.T.);
#4048=EDGE_CURVE('',#3305,#3290,#911,.T.);
#4049=EDGE_CURVE('',#3306,#3305,#351,.T.);
#4050=EDGE_CURVE('',#3291,#3306,#912,.T.);
#4051=EDGE_CURVE('',#3307,#3307,#913,.T.);
#4052=EDGE_CURVE('',#3307,#3300,#2341,.T.);
#4053=EDGE_CURVE('',#3308,#3275,#914,.T.);
#4054=EDGE_CURVE('',#3308,#3309,#352,.T.);
#4055=EDGE_CURVE('',#3306,#3309,#915,.T.);
#4056=EDGE_CURVE('',#3293,#3308,#916,.T.);
#4057=EDGE_CURVE('',#3309,#3292,#917,.T.);
#4058=EDGE_CURVE('',#3310,#3310,#918,.T.);
#4059=EDGE_CURVE('',#3311,#3311,#919,.T.);
#4060=EDGE_CURVE('',#3312,#3312,#920,.T.);
#4061=EDGE_CURVE('',#3312,#3310,#2342,.T.);
#4062=EDGE_CURVE('',#3313,#3313,#921,.T.);
#4063=EDGE_CURVE('',#3313,#3311,#2343,.T.);
#4064=EDGE_CURVE('',#3314,#3314,#922,.T.);
#4065=EDGE_CURVE('',#3315,#3315,#923,.T.);
#4066=EDGE_CURVE('',#3316,#3316,#924,.T.);
#4067=EDGE_CURVE('',#3316,#3314,#2344,.T.);
#4068=EDGE_CURVE('',#3317,#3317,#925,.T.);
#4069=EDGE_CURVE('',#3317,#3315,#2345,.T.);
#4070=EDGE_CURVE('',#3318,#3318,#926,.T.);
#4071=EDGE_CURVE('',#3318,#3319,#2346,.T.);
#4072=EDGE_CURVE('',#3319,#3319,#927,.T.);
#4073=EDGE_CURVE('',#3320,#3320,#928,.T.);
#4074=EDGE_CURVE('',#3320,#3321,#2347,.T.);
#4075=EDGE_CURVE('',#3321,#3321,#929,.T.);
#4076=EDGE_CURVE('',#3322,#3322,#930,.T.);
#4077=EDGE_CURVE('',#3322,#3323,#2348,.T.);
#4078=EDGE_CURVE('',#3323,#3323,#931,.T.);
#4079=EDGE_CURVE('',#3324,#3324,#932,.T.);
#4080=EDGE_CURVE('',#3324,#3325,#2349,.T.);
#4081=EDGE_CURVE('',#3325,#3325,#933,.T.);
#4082=EDGE_CURVE('',#3326,#3326,#934,.T.);
#4083=EDGE_CURVE('',#3326,#3327,#2350,.T.);
#4084=EDGE_CURVE('',#3327,#3327,#935,.T.);
#4085=EDGE_CURVE('',#3328,#3328,#936,.T.);
#4086=EDGE_CURVE('',#3328,#3329,#2351,.T.);
#4087=EDGE_CURVE('',#3329,#3329,#937,.T.);
#4088=ORIENTED_EDGE('',*,*,#3330,.F.);
#4089=ORIENTED_EDGE('',*,*,#3331,.T.);
#4090=ORIENTED_EDGE('',*,*,#3332,.F.);
#4091=ORIENTED_EDGE('',*,*,#3333,.F.);
#4092=ORIENTED_EDGE('',*,*,#3334,.F.);
#4093=ORIENTED_EDGE('',*,*,#3335,.T.);
#4094=ORIENTED_EDGE('',*,*,#3336,.F.);
#4095=ORIENTED_EDGE('',*,*,#3331,.F.);
#4096=ORIENTED_EDGE('',*,*,#3337,.F.);
#4097=ORIENTED_EDGE('',*,*,#3338,.T.);
#4098=ORIENTED_EDGE('',*,*,#3339,.F.);
#4099=ORIENTED_EDGE('',*,*,#3335,.F.);
#4100=ORIENTED_EDGE('',*,*,#3340,.F.);
#4101=ORIENTED_EDGE('',*,*,#3341,.T.);
#4102=ORIENTED_EDGE('',*,*,#3342,.F.);
#4103=ORIENTED_EDGE('',*,*,#3338,.F.);
#4104=ORIENTED_EDGE('',*,*,#3343,.F.);
#4105=ORIENTED_EDGE('',*,*,#3344,.T.);
#4106=ORIENTED_EDGE('',*,*,#3345,.F.);
#4107=ORIENTED_EDGE('',*,*,#3341,.F.);
#4108=ORIENTED_EDGE('',*,*,#3346,.F.);
#4109=ORIENTED_EDGE('',*,*,#3347,.T.);
#4110=ORIENTED_EDGE('',*,*,#3348,.F.);
#4111=ORIENTED_EDGE('',*,*,#3344,.F.);
#4112=ORIENTED_EDGE('',*,*,#3349,.F.);
#4113=ORIENTED_EDGE('',*,*,#3350,.T.);
#4114=ORIENTED_EDGE('',*,*,#3351,.F.);
#4115=ORIENTED_EDGE('',*,*,#3347,.F.);
#4116=ORIENTED_EDGE('',*,*,#3352,.F.);
#4117=ORIENTED_EDGE('',*,*,#3353,.T.);
#4118=ORIENTED_EDGE('',*,*,#3354,.F.);
#4119=ORIENTED_EDGE('',*,*,#3350,.F.);
#4120=ORIENTED_EDGE('',*,*,#3355,.F.);
#4121=ORIENTED_EDGE('',*,*,#3356,.F.);
#4122=ORIENTED_EDGE('',*,*,#3357,.F.);
#4123=ORIENTED_EDGE('',*,*,#3353,.F.);
#4124=ORIENTED_EDGE('',*,*,#3358,.F.);
#4125=ORIENTED_EDGE('',*,*,#3359,.T.);
#4126=ORIENTED_EDGE('',*,*,#3360,.F.);
#4127=ORIENTED_EDGE('',*,*,#3361,.F.);
#4128=ORIENTED_EDGE('',*,*,#3362,.F.);
#4129=ORIENTED_EDGE('',*,*,#3363,.T.);
#4130=ORIENTED_EDGE('',*,*,#3364,.F.);
#4131=ORIENTED_EDGE('',*,*,#3359,.F.);
#4132=ORIENTED_EDGE('',*,*,#3365,.F.);
#4133=ORIENTED_EDGE('',*,*,#3366,.T.);
#4134=ORIENTED_EDGE('',*,*,#3367,.F.);
#4135=ORIENTED_EDGE('',*,*,#3363,.F.);
#4136=ORIENTED_EDGE('',*,*,#3368,.F.);
#4137=ORIENTED_EDGE('',*,*,#3369,.T.);
#4138=ORIENTED_EDGE('',*,*,#3370,.F.);
#4139=ORIENTED_EDGE('',*,*,#3366,.F.);
#4140=ORIENTED_EDGE('',*,*,#3371,.F.);
#4141=ORIENTED_EDGE('',*,*,#3372,.T.);
#4142=ORIENTED_EDGE('',*,*,#3373,.F.);
#4143=ORIENTED_EDGE('',*,*,#3369,.F.);
#4144=ORIENTED_EDGE('',*,*,#3374,.F.);
#4145=ORIENTED_EDGE('',*,*,#3375,.T.);
#4146=ORIENTED_EDGE('',*,*,#3376,.F.);
#4147=ORIENTED_EDGE('',*,*,#3372,.F.);
#4148=ORIENTED_EDGE('',*,*,#3377,.F.);
#4149=ORIENTED_EDGE('',*,*,#3378,.T.);
#4150=ORIENTED_EDGE('',*,*,#3379,.F.);
#4151=ORIENTED_EDGE('',*,*,#3375,.F.);
#4152=ORIENTED_EDGE('',*,*,#3380,.F.);
#4153=ORIENTED_EDGE('',*,*,#3381,.T.);
#4154=ORIENTED_EDGE('',*,*,#3382,.F.);
#4155=ORIENTED_EDGE('',*,*,#3378,.F.);
#4156=ORIENTED_EDGE('',*,*,#3383,.F.);
#4157=ORIENTED_EDGE('',*,*,#3384,.F.);
#4158=ORIENTED_EDGE('',*,*,#3385,.F.);
#4159=ORIENTED_EDGE('',*,*,#3381,.F.);
#4160=ORIENTED_EDGE('',*,*,#3386,.F.);
#4161=ORIENTED_EDGE('',*,*,#3387,.T.);
#4162=ORIENTED_EDGE('',*,*,#3388,.F.);
#4163=ORIENTED_EDGE('',*,*,#3389,.F.);
#4164=ORIENTED_EDGE('',*,*,#3390,.F.);
#4165=ORIENTED_EDGE('',*,*,#3391,.T.);
#4166=ORIENTED_EDGE('',*,*,#3392,.F.);
#4167=ORIENTED_EDGE('',*,*,#3387,.F.);
#4168=ORIENTED_EDGE('',*,*,#3393,.F.);
#4169=ORIENTED_EDGE('',*,*,#3394,.T.);
#4170=ORIENTED_EDGE('',*,*,#3395,.F.);
#4171=ORIENTED_EDGE('',*,*,#3391,.F.);
#4172=ORIENTED_EDGE('',*,*,#3396,.F.);
#4173=ORIENTED_EDGE('',*,*,#3397,.T.);
#4174=ORIENTED_EDGE('',*,*,#3398,.F.);
#4175=ORIENTED_EDGE('',*,*,#3394,.F.);
#4176=ORIENTED_EDGE('',*,*,#3399,.F.);
#4177=ORIENTED_EDGE('',*,*,#3400,.T.);
#4178=ORIENTED_EDGE('',*,*,#3401,.F.);
#4179=ORIENTED_EDGE('',*,*,#3397,.F.);
#4180=ORIENTED_EDGE('',*,*,#3402,.F.);
#4181=ORIENTED_EDGE('',*,*,#3403,.T.);
#4182=ORIENTED_EDGE('',*,*,#3404,.F.);
#4183=ORIENTED_EDGE('',*,*,#3400,.F.);
#4184=ORIENTED_EDGE('',*,*,#3405,.F.);
#4185=ORIENTED_EDGE('',*,*,#3406,.T.);
#4186=ORIENTED_EDGE('',*,*,#3407,.F.);
#4187=ORIENTED_EDGE('',*,*,#3403,.F.);
#4188=ORIENTED_EDGE('',*,*,#3408,.F.);
#4189=ORIENTED_EDGE('',*,*,#3409,.T.);
#4190=ORIENTED_EDGE('',*,*,#3410,.F.);
#4191=ORIENTED_EDGE('',*,*,#3406,.F.);
#4192=ORIENTED_EDGE('',*,*,#3411,.F.);
#4193=ORIENTED_EDGE('',*,*,#3412,.F.);
#4194=ORIENTED_EDGE('',*,*,#3413,.F.);
#4195=ORIENTED_EDGE('',*,*,#3409,.F.);
#4196=ORIENTED_EDGE('',*,*,#3414,.F.);
#4197=ORIENTED_EDGE('',*,*,#3415,.T.);
#4198=ORIENTED_EDGE('',*,*,#3416,.F.);
#4199=ORIENTED_EDGE('',*,*,#3417,.F.);
#4200=ORIENTED_EDGE('',*,*,#3418,.F.);
#4201=ORIENTED_EDGE('',*,*,#3419,.T.);
#4202=ORIENTED_EDGE('',*,*,#3420,.F.);
#4203=ORIENTED_EDGE('',*,*,#3415,.F.);
#4204=ORIENTED_EDGE('',*,*,#3421,.F.);
#4205=ORIENTED_EDGE('',*,*,#3422,.T.);
#4206=ORIENTED_EDGE('',*,*,#3423,.F.);
#4207=ORIENTED_EDGE('',*,*,#3419,.F.);
#4208=ORIENTED_EDGE('',*,*,#3424,.F.);
#4209=ORIENTED_EDGE('',*,*,#3425,.T.);
#4210=ORIENTED_EDGE('',*,*,#3426,.F.);
#4211=ORIENTED_EDGE('',*,*,#3422,.F.);
#4212=ORIENTED_EDGE('',*,*,#3427,.F.);
#4213=ORIENTED_EDGE('',*,*,#3428,.T.);
#4214=ORIENTED_EDGE('',*,*,#3429,.F.);
#4215=ORIENTED_EDGE('',*,*,#3425,.F.);
#4216=ORIENTED_EDGE('',*,*,#3430,.F.);
#4217=ORIENTED_EDGE('',*,*,#3431,.T.);
#4218=ORIENTED_EDGE('',*,*,#3432,.F.);
#4219=ORIENTED_EDGE('',*,*,#3428,.F.);
#4220=ORIENTED_EDGE('',*,*,#3433,.F.);
#4221=ORIENTED_EDGE('',*,*,#3434,.T.);
#4222=ORIENTED_EDGE('',*,*,#3435,.F.);
#4223=ORIENTED_EDGE('',*,*,#3431,.F.);
#4224=ORIENTED_EDGE('',*,*,#3436,.F.);
#4225=ORIENTED_EDGE('',*,*,#3437,.T.);
#4226=ORIENTED_EDGE('',*,*,#3438,.F.);
#4227=ORIENTED_EDGE('',*,*,#3434,.F.);
#4228=ORIENTED_EDGE('',*,*,#3439,.F.);
#4229=ORIENTED_EDGE('',*,*,#3440,.F.);
#4230=ORIENTED_EDGE('',*,*,#3441,.F.);
#4231=ORIENTED_EDGE('',*,*,#3437,.F.);
#4232=ORIENTED_EDGE('',*,*,#3442,.F.);
#4233=ORIENTED_EDGE('',*,*,#3443,.T.);
#4234=ORIENTED_EDGE('',*,*,#3444,.F.);
#4235=ORIENTED_EDGE('',*,*,#3443,.F.);
#4236=ORIENTED_EDGE('',*,*,#3356,.T.);
#4237=ORIENTED_EDGE('',*,*,#3445,.T.);
#4238=ORIENTED_EDGE('',*,*,#3446,.T.);
#4239=ORIENTED_EDGE('',*,*,#3447,.F.);
#4240=ORIENTED_EDGE('',*,*,#3333,.T.);
#4241=ORIENTED_EDGE('',*,*,#3448,.F.);
#4242=ORIENTED_EDGE('',*,*,#3449,.F.);
#4243=ORIENTED_EDGE('',*,*,#3450,.T.);
#4244=ORIENTED_EDGE('',*,*,#3384,.T.);
#4245=ORIENTED_EDGE('',*,*,#3451,.T.);
#4246=ORIENTED_EDGE('',*,*,#3449,.T.);
#4247=ORIENTED_EDGE('',*,*,#3452,.F.);
#4248=ORIENTED_EDGE('',*,*,#3361,.T.);
#4249=ORIENTED_EDGE('',*,*,#3453,.F.);
#4250=ORIENTED_EDGE('',*,*,#3454,.F.);
#4251=ORIENTED_EDGE('',*,*,#3455,.T.);
#4252=ORIENTED_EDGE('',*,*,#3412,.T.);
#4253=ORIENTED_EDGE('',*,*,#3456,.T.);
#4254=ORIENTED_EDGE('',*,*,#3454,.T.);
#4255=ORIENTED_EDGE('',*,*,#3457,.F.);
#4256=ORIENTED_EDGE('',*,*,#3389,.T.);
#4257=ORIENTED_EDGE('',*,*,#3458,.F.);
#4258=ORIENTED_EDGE('',*,*,#3459,.F.);
#4259=ORIENTED_EDGE('',*,*,#3460,.T.);
#4260=ORIENTED_EDGE('',*,*,#3440,.T.);
#4261=ORIENTED_EDGE('',*,*,#3461,.T.);
#4262=ORIENTED_EDGE('',*,*,#3459,.T.);
#4263=ORIENTED_EDGE('',*,*,#3462,.F.);
#4264=ORIENTED_EDGE('',*,*,#3417,.T.);
#4265=ORIENTED_EDGE('',*,*,#3463,.F.);
#4266=ORIENTED_EDGE('',*,*,#3446,.F.);
#4267=ORIENTED_EDGE('',*,*,#3464,.T.);
#4268=ORIENTED_EDGE('',*,*,#3332,.T.);
#4269=ORIENTED_EDGE('',*,*,#3336,.T.);
#4270=ORIENTED_EDGE('',*,*,#3339,.T.);
#4271=ORIENTED_EDGE('',*,*,#3342,.T.);
#4272=ORIENTED_EDGE('',*,*,#3345,.T.);
#4273=ORIENTED_EDGE('',*,*,#3348,.T.);
#4274=ORIENTED_EDGE('',*,*,#3351,.T.);
#4275=ORIENTED_EDGE('',*,*,#3354,.T.);
#4276=ORIENTED_EDGE('',*,*,#3357,.T.);
#4277=ORIENTED_EDGE('',*,*,#3447,.T.);
#4278=ORIENTED_EDGE('',*,*,#3463,.T.);
#4279=ORIENTED_EDGE('',*,*,#3416,.T.);
#4280=ORIENTED_EDGE('',*,*,#3420,.T.);
#4281=ORIENTED_EDGE('',*,*,#3423,.T.);
#4282=ORIENTED_EDGE('',*,*,#3426,.T.);
#4283=ORIENTED_EDGE('',*,*,#3429,.T.);
#4284=ORIENTED_EDGE('',*,*,#3432,.T.);
#4285=ORIENTED_EDGE('',*,*,#3435,.T.);
#4286=ORIENTED_EDGE('',*,*,#3438,.T.);
#4287=ORIENTED_EDGE('',*,*,#3441,.T.);
#4288=ORIENTED_EDGE('',*,*,#3462,.T.);
#4289=ORIENTED_EDGE('',*,*,#3458,.T.);
#4290=ORIENTED_EDGE('',*,*,#3388,.T.);
#4291=ORIENTED_EDGE('',*,*,#3392,.T.);
#4292=ORIENTED_EDGE('',*,*,#3395,.T.);
#4293=ORIENTED_EDGE('',*,*,#3398,.T.);
#4294=ORIENTED_EDGE('',*,*,#3401,.T.);
#4295=ORIENTED_EDGE('',*,*,#3404,.T.);
#4296=ORIENTED_EDGE('',*,*,#3407,.T.);
#4297=ORIENTED_EDGE('',*,*,#3410,.T.);
#4298=ORIENTED_EDGE('',*,*,#3413,.T.);
#4299=ORIENTED_EDGE('',*,*,#3457,.T.);
#4300=ORIENTED_EDGE('',*,*,#3453,.T.);
#4301=ORIENTED_EDGE('',*,*,#3360,.T.);
#4302=ORIENTED_EDGE('',*,*,#3364,.T.);
#4303=ORIENTED_EDGE('',*,*,#3367,.T.);
#4304=ORIENTED_EDGE('',*,*,#3370,.T.);
#4305=ORIENTED_EDGE('',*,*,#3373,.T.);
#4306=ORIENTED_EDGE('',*,*,#3376,.T.);
#4307=ORIENTED_EDGE('',*,*,#3379,.T.);
#4308=ORIENTED_EDGE('',*,*,#3382,.T.);
#4309=ORIENTED_EDGE('',*,*,#3385,.T.);
#4310=ORIENTED_EDGE('',*,*,#3452,.T.);
#4311=ORIENTED_EDGE('',*,*,#3448,.T.);
#4312=ORIENTED_EDGE('',*,*,#3444,.T.);
#4313=ORIENTED_EDGE('',*,*,#3330,.T.);
#4314=ORIENTED_EDGE('',*,*,#3450,.F.);
#4315=ORIENTED_EDGE('',*,*,#3451,.F.);
#4316=ORIENTED_EDGE('',*,*,#3383,.T.);
#4317=ORIENTED_EDGE('',*,*,#3380,.T.);
#4318=ORIENTED_EDGE('',*,*,#3377,.T.);
#4319=ORIENTED_EDGE('',*,*,#3374,.T.);
#4320=ORIENTED_EDGE('',*,*,#3371,.T.);
#4321=ORIENTED_EDGE('',*,*,#3368,.T.);
#4322=ORIENTED_EDGE('',*,*,#3365,.T.);
#4323=ORIENTED_EDGE('',*,*,#3362,.T.);
#4324=ORIENTED_EDGE('',*,*,#3358,.T.);
#4325=ORIENTED_EDGE('',*,*,#3455,.F.);
#4326=ORIENTED_EDGE('',*,*,#3456,.F.);
#4327=ORIENTED_EDGE('',*,*,#3411,.T.);
#4328=ORIENTED_EDGE('',*,*,#3408,.T.);
#4329=ORIENTED_EDGE('',*,*,#3405,.T.);
#4330=ORIENTED_EDGE('',*,*,#3402,.T.);
#4331=ORIENTED_EDGE('',*,*,#3399,.T.);
#4332=ORIENTED_EDGE('',*,*,#3396,.T.);
#4333=ORIENTED_EDGE('',*,*,#3393,.T.);
#4334=ORIENTED_EDGE('',*,*,#3390,.T.);
#4335=ORIENTED_EDGE('',*,*,#3386,.T.);
#4336=ORIENTED_EDGE('',*,*,#3460,.F.);
#4337=ORIENTED_EDGE('',*,*,#3461,.F.);
#4338=ORIENTED_EDGE('',*,*,#3439,.T.);
#4339=ORIENTED_EDGE('',*,*,#3436,.T.);
#4340=ORIENTED_EDGE('',*,*,#3433,.T.);
#4341=ORIENTED_EDGE('',*,*,#3430,.T.);
#4342=ORIENTED_EDGE('',*,*,#3427,.T.);
#4343=ORIENTED_EDGE('',*,*,#3424,.T.);
#4344=ORIENTED_EDGE('',*,*,#3421,.T.);
#4345=ORIENTED_EDGE('',*,*,#3418,.T.);
#4346=ORIENTED_EDGE('',*,*,#3414,.T.);
#4347=ORIENTED_EDGE('',*,*,#3464,.F.);
#4348=ORIENTED_EDGE('',*,*,#3445,.F.);
#4349=ORIENTED_EDGE('',*,*,#3355,.T.);
#4350=ORIENTED_EDGE('',*,*,#3352,.T.);
#4351=ORIENTED_EDGE('',*,*,#3349,.T.);
#4352=ORIENTED_EDGE('',*,*,#3346,.T.);
#4353=ORIENTED_EDGE('',*,*,#3343,.T.);
#4354=ORIENTED_EDGE('',*,*,#3340,.T.);
#4355=ORIENTED_EDGE('',*,*,#3337,.T.);
#4356=ORIENTED_EDGE('',*,*,#3334,.T.);
#4357=ORIENTED_EDGE('',*,*,#3442,.T.);
#4358=ORIENTED_EDGE('',*,*,#3465,.F.);
#4359=ORIENTED_EDGE('',*,*,#3466,.T.);
#4360=ORIENTED_EDGE('',*,*,#3467,.F.);
#4361=ORIENTED_EDGE('',*,*,#3466,.F.);
#4362=ORIENTED_EDGE('',*,*,#3468,.F.);
#4363=ORIENTED_EDGE('',*,*,#3469,.T.);
#4364=ORIENTED_EDGE('',*,*,#3470,.F.);
#4365=ORIENTED_EDGE('',*,*,#3469,.F.);
#4366=ORIENTED_EDGE('',*,*,#3471,.F.);
#4367=ORIENTED_EDGE('',*,*,#3472,.T.);
#4368=ORIENTED_EDGE('',*,*,#3473,.F.);
#4369=ORIENTED_EDGE('',*,*,#3472,.F.);
#4370=ORIENTED_EDGE('',*,*,#3474,.F.);
#4371=ORIENTED_EDGE('',*,*,#3475,.T.);
#4372=ORIENTED_EDGE('',*,*,#3476,.F.);
#4373=ORIENTED_EDGE('',*,*,#3475,.F.);
#4374=ORIENTED_EDGE('',*,*,#3477,.F.);
#4375=ORIENTED_EDGE('',*,*,#3478,.T.);
#4376=ORIENTED_EDGE('',*,*,#3479,.F.);
#4377=ORIENTED_EDGE('',*,*,#3478,.F.);
#4378=ORIENTED_EDGE('',*,*,#3480,.F.);
#4379=ORIENTED_EDGE('',*,*,#3481,.T.);
#4380=ORIENTED_EDGE('',*,*,#3482,.F.);
#4381=ORIENTED_EDGE('',*,*,#3481,.F.);
#4382=ORIENTED_EDGE('',*,*,#3483,.F.);
#4383=ORIENTED_EDGE('',*,*,#3484,.T.);
#4384=ORIENTED_EDGE('',*,*,#3485,.F.);
#4385=ORIENTED_EDGE('',*,*,#3484,.F.);
#4386=ORIENTED_EDGE('',*,*,#3486,.F.);
#4387=ORIENTED_EDGE('',*,*,#3487,.T.);
#4388=ORIENTED_EDGE('',*,*,#3488,.F.);
#4389=ORIENTED_EDGE('',*,*,#3487,.F.);
#4390=ORIENTED_EDGE('',*,*,#3489,.F.);
#4391=ORIENTED_EDGE('',*,*,#3490,.T.);
#4392=ORIENTED_EDGE('',*,*,#3491,.F.);
#4393=ORIENTED_EDGE('',*,*,#3490,.F.);
#4394=ORIENTED_EDGE('',*,*,#3492,.F.);
#4395=ORIENTED_EDGE('',*,*,#3493,.T.);
#4396=ORIENTED_EDGE('',*,*,#3494,.F.);
#4397=ORIENTED_EDGE('',*,*,#3493,.F.);
#4398=ORIENTED_EDGE('',*,*,#3495,.F.);
#4399=ORIENTED_EDGE('',*,*,#3496,.T.);
#4400=ORIENTED_EDGE('',*,*,#3497,.F.);
#4401=ORIENTED_EDGE('',*,*,#3496,.F.);
#4402=ORIENTED_EDGE('',*,*,#3498,.F.);
#4403=ORIENTED_EDGE('',*,*,#3499,.T.);
#4404=ORIENTED_EDGE('',*,*,#3500,.F.);
#4405=ORIENTED_EDGE('',*,*,#3499,.F.);
#4406=ORIENTED_EDGE('',*,*,#3501,.T.);
#4407=ORIENTED_EDGE('',*,*,#3502,.T.);
#4408=ORIENTED_EDGE('',*,*,#3503,.F.);
#4409=ORIENTED_EDGE('',*,*,#3504,.F.);
#4410=ORIENTED_EDGE('',*,*,#3505,.T.);
#4411=ORIENTED_EDGE('',*,*,#3504,.T.);
#4412=ORIENTED_EDGE('',*,*,#3506,.F.);
#4413=ORIENTED_EDGE('',*,*,#3507,.F.);
#4414=ORIENTED_EDGE('',*,*,#3508,.T.);
#4415=ORIENTED_EDGE('',*,*,#3507,.T.);
#4416=ORIENTED_EDGE('',*,*,#3509,.F.);
#4417=ORIENTED_EDGE('',*,*,#3510,.F.);
#4418=ORIENTED_EDGE('',*,*,#3511,.T.);
#4419=ORIENTED_EDGE('',*,*,#3510,.T.);
#4420=ORIENTED_EDGE('',*,*,#3512,.F.);
#4421=ORIENTED_EDGE('',*,*,#3502,.F.);
#4422=ORIENTED_EDGE('',*,*,#3512,.T.);
#4423=ORIENTED_EDGE('',*,*,#3509,.T.);
#4424=ORIENTED_EDGE('',*,*,#3506,.T.);
#4425=ORIENTED_EDGE('',*,*,#3503,.T.);
#4426=ORIENTED_EDGE('',*,*,#3473,.T.);
#4427=ORIENTED_EDGE('',*,*,#3476,.T.);
#4428=ORIENTED_EDGE('',*,*,#3485,.T.);
#4429=ORIENTED_EDGE('',*,*,#3488,.T.);
#4430=ORIENTED_EDGE('',*,*,#3491,.T.);
#4431=ORIENTED_EDGE('',*,*,#3494,.T.);
#4432=ORIENTED_EDGE('',*,*,#3497,.T.);
#4433=ORIENTED_EDGE('',*,*,#3500,.T.);
#4434=ORIENTED_EDGE('',*,*,#3482,.T.);
#4435=ORIENTED_EDGE('',*,*,#3479,.T.);
#4436=ORIENTED_EDGE('',*,*,#3470,.T.);
#4437=ORIENTED_EDGE('',*,*,#3467,.T.);
#4438=ORIENTED_EDGE('',*,*,#3511,.F.);
#4439=ORIENTED_EDGE('',*,*,#3501,.F.);
#4440=ORIENTED_EDGE('',*,*,#3505,.F.);
#4441=ORIENTED_EDGE('',*,*,#3508,.F.);
#4442=ORIENTED_EDGE('',*,*,#3471,.T.);
#4443=ORIENTED_EDGE('',*,*,#3474,.T.);
#4444=ORIENTED_EDGE('',*,*,#3483,.T.);
#4445=ORIENTED_EDGE('',*,*,#3486,.T.);
#4446=ORIENTED_EDGE('',*,*,#3489,.T.);
#4447=ORIENTED_EDGE('',*,*,#3492,.T.);
#4448=ORIENTED_EDGE('',*,*,#3495,.T.);
#4449=ORIENTED_EDGE('',*,*,#3498,.T.);
#4450=ORIENTED_EDGE('',*,*,#3480,.T.);
#4451=ORIENTED_EDGE('',*,*,#3477,.T.);
#4452=ORIENTED_EDGE('',*,*,#3468,.T.);
#4453=ORIENTED_EDGE('',*,*,#3465,.T.);
#4454=ORIENTED_EDGE('',*,*,#3513,.F.);
#4455=ORIENTED_EDGE('',*,*,#3514,.F.);
#4456=ORIENTED_EDGE('',*,*,#3515,.F.);
#4457=ORIENTED_EDGE('',*,*,#3516,.F.);
#4458=ORIENTED_EDGE('',*,*,#3515,.T.);
#4459=ORIENTED_EDGE('',*,*,#3517,.T.);
#4460=ORIENTED_EDGE('',*,*,#3518,.F.);
#4461=ORIENTED_EDGE('',*,*,#3519,.F.);
#4462=ORIENTED_EDGE('',*,*,#3520,.T.);
#4463=ORIENTED_EDGE('',*,*,#3521,.T.);
#4464=ORIENTED_EDGE('',*,*,#3522,.T.);
#4465=ORIENTED_EDGE('',*,*,#3518,.T.);
#4466=ORIENTED_EDGE('',*,*,#3523,.T.);
#4467=ORIENTED_EDGE('',*,*,#3520,.F.);
#4468=ORIENTED_EDGE('',*,*,#3517,.F.);
#4469=ORIENTED_EDGE('',*,*,#3514,.T.);
#4470=ORIENTED_EDGE('',*,*,#3524,.F.);
#4471=ORIENTED_EDGE('',*,*,#3525,.F.);
#4472=ORIENTED_EDGE('',*,*,#3526,.T.);
#4473=ORIENTED_EDGE('',*,*,#3527,.F.);
#4474=ORIENTED_EDGE('',*,*,#3528,.T.);
#4475=ORIENTED_EDGE('',*,*,#3529,.T.);
#4476=ORIENTED_EDGE('',*,*,#3530,.T.);
#4477=ORIENTED_EDGE('',*,*,#3531,.T.);
#4478=ORIENTED_EDGE('',*,*,#3532,.T.);
#4479=ORIENTED_EDGE('',*,*,#3521,.F.);
#4480=ORIENTED_EDGE('',*,*,#3530,.F.);
#4481=ORIENTED_EDGE('',*,*,#3533,.F.);
#4482=ORIENTED_EDGE('',*,*,#3534,.F.);
#4483=ORIENTED_EDGE('',*,*,#3531,.F.);
#4484=ORIENTED_EDGE('',*,*,#3529,.F.);
#4485=ORIENTED_EDGE('',*,*,#3522,.F.);
#4486=ORIENTED_EDGE('',*,*,#3532,.F.);
#4487=ORIENTED_EDGE('',*,*,#3534,.T.);
#4488=ORIENTED_EDGE('',*,*,#3535,.F.);
#4489=ORIENTED_EDGE('',*,*,#3536,.F.);
#4490=ORIENTED_EDGE('',*,*,#3537,.T.);
#4491=ORIENTED_EDGE('',*,*,#3538,.F.);
#4492=ORIENTED_EDGE('',*,*,#3539,.T.);
#4493=ORIENTED_EDGE('',*,*,#3516,.T.);
#4494=ORIENTED_EDGE('',*,*,#3519,.T.);
#4495=ORIENTED_EDGE('',*,*,#3533,.T.);
#4496=ORIENTED_EDGE('',*,*,#3528,.F.);
#4497=ORIENTED_EDGE('',*,*,#3540,.F.);
#4498=ORIENTED_EDGE('',*,*,#3535,.T.);
#4499=ORIENTED_EDGE('',*,*,#3536,.T.);
#4500=ORIENTED_EDGE('',*,*,#3540,.T.);
#4501=ORIENTED_EDGE('',*,*,#3527,.T.);
#4502=ORIENTED_EDGE('',*,*,#3541,.T.);
#4503=ORIENTED_EDGE('',*,*,#3542,.T.);
#4504=ORIENTED_EDGE('',*,*,#3543,.T.);
#4505=ORIENTED_EDGE('',*,*,#3542,.F.);
#4506=ORIENTED_EDGE('',*,*,#3544,.F.);
#4507=ORIENTED_EDGE('',*,*,#3545,.T.);
#4508=ORIENTED_EDGE('',*,*,#3523,.F.);
#4509=ORIENTED_EDGE('',*,*,#3545,.F.);
#4510=ORIENTED_EDGE('',*,*,#3546,.F.);
#4511=ORIENTED_EDGE('',*,*,#3547,.F.);
#4512=ORIENTED_EDGE('',*,*,#3548,.F.);
#4513=ORIENTED_EDGE('',*,*,#3541,.F.);
#4514=ORIENTED_EDGE('',*,*,#3526,.F.);
#4515=ORIENTED_EDGE('',*,*,#3549,.F.);
#4516=ORIENTED_EDGE('',*,*,#3546,.T.);
#4517=ORIENTED_EDGE('',*,*,#3544,.T.);
#4518=ORIENTED_EDGE('',*,*,#3543,.F.);
#4519=ORIENTED_EDGE('',*,*,#3548,.T.);
#4520=ORIENTED_EDGE('',*,*,#3550,.F.);
#4521=ORIENTED_EDGE('',*,*,#3537,.F.);
#4522=ORIENTED_EDGE('',*,*,#3525,.T.);
#4523=ORIENTED_EDGE('',*,*,#3551,.T.);
#4524=ORIENTED_EDGE('',*,*,#3538,.T.);
#4525=ORIENTED_EDGE('',*,*,#3550,.T.);
#4526=ORIENTED_EDGE('',*,*,#3547,.T.);
#4527=ORIENTED_EDGE('',*,*,#3549,.T.);
#4528=ORIENTED_EDGE('',*,*,#3513,.T.);
#4529=ORIENTED_EDGE('',*,*,#3539,.F.);
#4530=ORIENTED_EDGE('',*,*,#3551,.F.);
#4531=ORIENTED_EDGE('',*,*,#3524,.T.);
#4532=ORIENTED_EDGE('',*,*,#3552,.T.);
#4533=ORIENTED_EDGE('',*,*,#3553,.T.);
#4534=ORIENTED_EDGE('',*,*,#3554,.T.);
#4535=ORIENTED_EDGE('',*,*,#3553,.F.);
#4536=ORIENTED_EDGE('',*,*,#3554,.F.);
#4537=ORIENTED_EDGE('',*,*,#3555,.T.);
#4538=ORIENTED_EDGE('',*,*,#3556,.T.);
#4539=ORIENTED_EDGE('',*,*,#3555,.F.);
#4540=ORIENTED_EDGE('',*,*,#3557,.T.);
#4541=ORIENTED_EDGE('',*,*,#3552,.F.);
#4542=ORIENTED_EDGE('',*,*,#3557,.F.);
#4543=ORIENTED_EDGE('',*,*,#3558,.T.);
#4544=ORIENTED_EDGE('',*,*,#3559,.T.);
#4545=ORIENTED_EDGE('',*,*,#3558,.F.);
#4546=ORIENTED_EDGE('',*,*,#3559,.F.);
#4547=ORIENTED_EDGE('',*,*,#3556,.F.);
#4548=ORIENTED_EDGE('',*,*,#3560,.T.);
#4549=ORIENTED_EDGE('',*,*,#3561,.T.);
#4550=ORIENTED_EDGE('',*,*,#3562,.F.);
#4551=ORIENTED_EDGE('',*,*,#3563,.F.);
#4552=ORIENTED_EDGE('',*,*,#3564,.T.);
#4553=ORIENTED_EDGE('',*,*,#3563,.T.);
#4554=ORIENTED_EDGE('',*,*,#3565,.F.);
#4555=ORIENTED_EDGE('',*,*,#3566,.F.);
#4556=ORIENTED_EDGE('',*,*,#3567,.T.);
#4557=ORIENTED_EDGE('',*,*,#3566,.T.);
#4558=ORIENTED_EDGE('',*,*,#3568,.F.);
#4559=ORIENTED_EDGE('',*,*,#3569,.F.);
#4560=ORIENTED_EDGE('',*,*,#3570,.T.);
#4561=ORIENTED_EDGE('',*,*,#3569,.T.);
#4562=ORIENTED_EDGE('',*,*,#3571,.F.);
#4563=ORIENTED_EDGE('',*,*,#3561,.F.);
#4564=ORIENTED_EDGE('',*,*,#3571,.T.);
#4565=ORIENTED_EDGE('',*,*,#3568,.T.);
#4566=ORIENTED_EDGE('',*,*,#3565,.T.);
#4567=ORIENTED_EDGE('',*,*,#3562,.T.);
#4568=ORIENTED_EDGE('',*,*,#3570,.F.);
#4569=ORIENTED_EDGE('',*,*,#3560,.F.);
#4570=ORIENTED_EDGE('',*,*,#3564,.F.);
#4571=ORIENTED_EDGE('',*,*,#3567,.F.);
#4572=ORIENTED_EDGE('',*,*,#3572,.T.);
#4573=ORIENTED_EDGE('',*,*,#3573,.T.);
#4574=ORIENTED_EDGE('',*,*,#3574,.F.);
#4575=ORIENTED_EDGE('',*,*,#3575,.F.);
#4576=ORIENTED_EDGE('',*,*,#3576,.T.);
#4577=ORIENTED_EDGE('',*,*,#3575,.T.);
#4578=ORIENTED_EDGE('',*,*,#3577,.F.);
#4579=ORIENTED_EDGE('',*,*,#3578,.F.);
#4580=ORIENTED_EDGE('',*,*,#3579,.T.);
#4581=ORIENTED_EDGE('',*,*,#3578,.T.);
#4582=ORIENTED_EDGE('',*,*,#3580,.F.);
#4583=ORIENTED_EDGE('',*,*,#3581,.F.);
#4584=ORIENTED_EDGE('',*,*,#3582,.T.);
#4585=ORIENTED_EDGE('',*,*,#3581,.T.);
#4586=ORIENTED_EDGE('',*,*,#3583,.F.);
#4587=ORIENTED_EDGE('',*,*,#3573,.F.);
#4588=ORIENTED_EDGE('',*,*,#3583,.T.);
#4589=ORIENTED_EDGE('',*,*,#3580,.T.);
#4590=ORIENTED_EDGE('',*,*,#3577,.T.);
#4591=ORIENTED_EDGE('',*,*,#3574,.T.);
#4592=ORIENTED_EDGE('',*,*,#3582,.F.);
#4593=ORIENTED_EDGE('',*,*,#3572,.F.);
#4594=ORIENTED_EDGE('',*,*,#3576,.F.);
#4595=ORIENTED_EDGE('',*,*,#3579,.F.);
#4596=ORIENTED_EDGE('',*,*,#3584,.F.);
#4597=ORIENTED_EDGE('',*,*,#3585,.T.);
#4598=ORIENTED_EDGE('',*,*,#3586,.F.);
#4599=ORIENTED_EDGE('',*,*,#3585,.F.);
#4600=ORIENTED_EDGE('',*,*,#3587,.F.);
#4601=ORIENTED_EDGE('',*,*,#3588,.T.);
#4602=ORIENTED_EDGE('',*,*,#3589,.F.);
#4603=ORIENTED_EDGE('',*,*,#3588,.F.);
#4604=ORIENTED_EDGE('',*,*,#3590,.F.);
#4605=ORIENTED_EDGE('',*,*,#3591,.F.);
#4606=ORIENTED_EDGE('',*,*,#3592,.F.);
#4607=ORIENTED_EDGE('',*,*,#3593,.F.);
#4608=ORIENTED_EDGE('',*,*,#3592,.T.);
#4609=ORIENTED_EDGE('',*,*,#3594,.F.);
#4610=ORIENTED_EDGE('',*,*,#3595,.F.);
#4611=ORIENTED_EDGE('',*,*,#3596,.T.);
#4612=ORIENTED_EDGE('',*,*,#3597,.T.);
#4613=ORIENTED_EDGE('',*,*,#3598,.F.);
#4614=ORIENTED_EDGE('',*,*,#3599,.T.);
#4615=ORIENTED_EDGE('',*,*,#3600,.T.);
#4616=ORIENTED_EDGE('',*,*,#3591,.T.);
#4617=ORIENTED_EDGE('',*,*,#3601,.T.);
#4618=ORIENTED_EDGE('',*,*,#3602,.T.);
#4619=ORIENTED_EDGE('',*,*,#3594,.T.);
#4620=ORIENTED_EDGE('',*,*,#3603,.F.);
#4621=ORIENTED_EDGE('',*,*,#3604,.T.);
#4622=ORIENTED_EDGE('',*,*,#3600,.F.);
#4623=ORIENTED_EDGE('',*,*,#3604,.F.);
#4624=ORIENTED_EDGE('',*,*,#3605,.F.);
#4625=ORIENTED_EDGE('',*,*,#3606,.T.);
#4626=ORIENTED_EDGE('',*,*,#3599,.F.);
#4627=ORIENTED_EDGE('',*,*,#3606,.F.);
#4628=ORIENTED_EDGE('',*,*,#3607,.F.);
#4629=ORIENTED_EDGE('',*,*,#3608,.T.);
#4630=ORIENTED_EDGE('',*,*,#3609,.F.);
#4631=ORIENTED_EDGE('',*,*,#3610,.F.);
#4632=ORIENTED_EDGE('',*,*,#3586,.T.);
#4633=ORIENTED_EDGE('',*,*,#3589,.T.);
#4634=ORIENTED_EDGE('',*,*,#3607,.T.);
#4635=ORIENTED_EDGE('',*,*,#3611,.T.);
#4636=ORIENTED_EDGE('',*,*,#3612,.T.);
#4637=ORIENTED_EDGE('',*,*,#3613,.T.);
#4638=ORIENTED_EDGE('',*,*,#3614,.T.);
#4639=ORIENTED_EDGE('',*,*,#3595,.T.);
#4640=ORIENTED_EDGE('',*,*,#3602,.F.);
#4641=ORIENTED_EDGE('',*,*,#3615,.F.);
#4642=ORIENTED_EDGE('',*,*,#3608,.F.);
#4643=ORIENTED_EDGE('',*,*,#3613,.F.);
#4644=ORIENTED_EDGE('',*,*,#3590,.T.);
#4645=ORIENTED_EDGE('',*,*,#3616,.F.);
#4646=ORIENTED_EDGE('',*,*,#3617,.F.);
#4647=ORIENTED_EDGE('',*,*,#3609,.T.);
#4648=ORIENTED_EDGE('',*,*,#3615,.T.);
#4649=ORIENTED_EDGE('',*,*,#3601,.F.);
#4650=ORIENTED_EDGE('',*,*,#3603,.T.);
#4651=ORIENTED_EDGE('',*,*,#3605,.T.);
#4652=ORIENTED_EDGE('',*,*,#3618,.T.);
#4653=ORIENTED_EDGE('',*,*,#3611,.F.);
#4654=ORIENTED_EDGE('',*,*,#3610,.T.);
#4655=ORIENTED_EDGE('',*,*,#3617,.T.);
#4656=ORIENTED_EDGE('',*,*,#3619,.F.);
#4657=ORIENTED_EDGE('',*,*,#3597,.F.);
#4658=ORIENTED_EDGE('',*,*,#3593,.T.);
#4659=ORIENTED_EDGE('',*,*,#3598,.T.);
#4660=ORIENTED_EDGE('',*,*,#3619,.T.);
#4661=ORIENTED_EDGE('',*,*,#3616,.T.);
#4662=ORIENTED_EDGE('',*,*,#3618,.F.);
#4663=ORIENTED_EDGE('',*,*,#3596,.F.);
#4664=ORIENTED_EDGE('',*,*,#3614,.F.);
#4665=ORIENTED_EDGE('',*,*,#3612,.F.);
#4666=ORIENTED_EDGE('',*,*,#3584,.T.);
#4667=ORIENTED_EDGE('',*,*,#3587,.T.);
#4668=ORIENTED_EDGE('',*,*,#3620,.F.);
#4669=ORIENTED_EDGE('',*,*,#3621,.T.);
#4670=ORIENTED_EDGE('',*,*,#3622,.F.);
#4671=ORIENTED_EDGE('',*,*,#3621,.F.);
#4672=ORIENTED_EDGE('',*,*,#3620,.T.);
#4673=ORIENTED_EDGE('',*,*,#3623,.T.);
#4674=ORIENTED_EDGE('',*,*,#3624,.F.);
#4675=ORIENTED_EDGE('',*,*,#3623,.F.);
#4676=ORIENTED_EDGE('',*,*,#3625,.T.);
#4677=ORIENTED_EDGE('',*,*,#3626,.T.);
#4678=ORIENTED_EDGE('',*,*,#3625,.F.);
#4679=ORIENTED_EDGE('',*,*,#3626,.F.);
#4680=ORIENTED_EDGE('',*,*,#3627,.F.);
#4681=ORIENTED_EDGE('',*,*,#3628,.T.);
#4682=ORIENTED_EDGE('',*,*,#3624,.T.);
#4683=ORIENTED_EDGE('',*,*,#3628,.F.);
#4684=ORIENTED_EDGE('',*,*,#3627,.T.);
#4685=ORIENTED_EDGE('',*,*,#3622,.T.);
#4686=ORIENTED_EDGE('',*,*,#3629,.F.);
#4687=ORIENTED_EDGE('',*,*,#3630,.T.);
#4688=ORIENTED_EDGE('',*,*,#3631,.T.);
#4689=ORIENTED_EDGE('',*,*,#3630,.F.);
#4690=ORIENTED_EDGE('',*,*,#3632,.F.);
#4691=ORIENTED_EDGE('',*,*,#3633,.T.);
#4692=ORIENTED_EDGE('',*,*,#3634,.T.);
#4693=ORIENTED_EDGE('',*,*,#3633,.F.);
#4694=ORIENTED_EDGE('',*,*,#3632,.T.);
#4695=ORIENTED_EDGE('',*,*,#3629,.T.);
#4696=ORIENTED_EDGE('',*,*,#3634,.F.);
#4697=ORIENTED_EDGE('',*,*,#3631,.F.);
#4698=ORIENTED_EDGE('',*,*,#3635,.F.);
#4699=ORIENTED_EDGE('',*,*,#3636,.T.);
#4700=ORIENTED_EDGE('',*,*,#3637,.T.);
#4701=ORIENTED_EDGE('',*,*,#3636,.F.);
#4702=ORIENTED_EDGE('',*,*,#3638,.F.);
#4703=ORIENTED_EDGE('',*,*,#3639,.T.);
#4704=ORIENTED_EDGE('',*,*,#3640,.T.);
#4705=ORIENTED_EDGE('',*,*,#3639,.F.);
#4706=ORIENTED_EDGE('',*,*,#3638,.T.);
#4707=ORIENTED_EDGE('',*,*,#3635,.T.);
#4708=ORIENTED_EDGE('',*,*,#3640,.F.);
#4709=ORIENTED_EDGE('',*,*,#3637,.F.);
#4710=ORIENTED_EDGE('',*,*,#3641,.F.);
#4711=ORIENTED_EDGE('',*,*,#3642,.T.);
#4712=ORIENTED_EDGE('',*,*,#3643,.T.);
#4713=ORIENTED_EDGE('',*,*,#3642,.F.);
#4714=ORIENTED_EDGE('',*,*,#3644,.F.);
#4715=ORIENTED_EDGE('',*,*,#3645,.T.);
#4716=ORIENTED_EDGE('',*,*,#3646,.T.);
#4717=ORIENTED_EDGE('',*,*,#3645,.F.);
#4718=ORIENTED_EDGE('',*,*,#3644,.T.);
#4719=ORIENTED_EDGE('',*,*,#3641,.T.);
#4720=ORIENTED_EDGE('',*,*,#3646,.F.);
#4721=ORIENTED_EDGE('',*,*,#3643,.F.);
#4722=ORIENTED_EDGE('',*,*,#3647,.F.);
#4723=ORIENTED_EDGE('',*,*,#3648,.T.);
#4724=ORIENTED_EDGE('',*,*,#3649,.F.);
#4725=ORIENTED_EDGE('',*,*,#3648,.F.);
#4726=ORIENTED_EDGE('',*,*,#3647,.T.);
#4727=ORIENTED_EDGE('',*,*,#3650,.T.);
#4728=ORIENTED_EDGE('',*,*,#3651,.F.);
#4729=ORIENTED_EDGE('',*,*,#3650,.F.);
#4730=ORIENTED_EDGE('',*,*,#3652,.T.);
#4731=ORIENTED_EDGE('',*,*,#3653,.T.);
#4732=ORIENTED_EDGE('',*,*,#3652,.F.);
#4733=ORIENTED_EDGE('',*,*,#3653,.F.);
#4734=ORIENTED_EDGE('',*,*,#3654,.F.);
#4735=ORIENTED_EDGE('',*,*,#3655,.T.);
#4736=ORIENTED_EDGE('',*,*,#3651,.T.);
#4737=ORIENTED_EDGE('',*,*,#3655,.F.);
#4738=ORIENTED_EDGE('',*,*,#3654,.T.);
#4739=ORIENTED_EDGE('',*,*,#3649,.T.);
#4740=ORIENTED_EDGE('',*,*,#3656,.F.);
#4741=ORIENTED_EDGE('',*,*,#3657,.T.);
#4742=ORIENTED_EDGE('',*,*,#3658,.T.);
#4743=ORIENTED_EDGE('',*,*,#3657,.F.);
#4744=ORIENTED_EDGE('',*,*,#3659,.F.);
#4745=ORIENTED_EDGE('',*,*,#3660,.T.);
#4746=ORIENTED_EDGE('',*,*,#3661,.T.);
#4747=ORIENTED_EDGE('',*,*,#3660,.F.);
#4748=ORIENTED_EDGE('',*,*,#3659,.T.);
#4749=ORIENTED_EDGE('',*,*,#3656,.T.);
#4750=ORIENTED_EDGE('',*,*,#3661,.F.);
#4751=ORIENTED_EDGE('',*,*,#3658,.F.);
#4752=ORIENTED_EDGE('',*,*,#3662,.F.);
#4753=ORIENTED_EDGE('',*,*,#3663,.T.);
#4754=ORIENTED_EDGE('',*,*,#3664,.T.);
#4755=ORIENTED_EDGE('',*,*,#3663,.F.);
#4756=ORIENTED_EDGE('',*,*,#3665,.F.);
#4757=ORIENTED_EDGE('',*,*,#3666,.T.);
#4758=ORIENTED_EDGE('',*,*,#3667,.T.);
#4759=ORIENTED_EDGE('',*,*,#3666,.F.);
#4760=ORIENTED_EDGE('',*,*,#3665,.T.);
#4761=ORIENTED_EDGE('',*,*,#3662,.T.);
#4762=ORIENTED_EDGE('',*,*,#3667,.F.);
#4763=ORIENTED_EDGE('',*,*,#3664,.F.);
#4764=ORIENTED_EDGE('',*,*,#3668,.F.);
#4765=ORIENTED_EDGE('',*,*,#3669,.T.);
#4766=ORIENTED_EDGE('',*,*,#3670,.F.);
#4767=ORIENTED_EDGE('',*,*,#3669,.F.);
#4768=ORIENTED_EDGE('',*,*,#3671,.F.);
#4769=ORIENTED_EDGE('',*,*,#3672,.T.);
#4770=ORIENTED_EDGE('',*,*,#3673,.F.);
#4771=ORIENTED_EDGE('',*,*,#3672,.F.);
#4772=ORIENTED_EDGE('',*,*,#3674,.F.);
#4773=ORIENTED_EDGE('',*,*,#3675,.F.);
#4774=ORIENTED_EDGE('',*,*,#3676,.F.);
#4775=ORIENTED_EDGE('',*,*,#3677,.F.);
#4776=ORIENTED_EDGE('',*,*,#3676,.T.);
#4777=ORIENTED_EDGE('',*,*,#3678,.F.);
#4778=ORIENTED_EDGE('',*,*,#3679,.F.);
#4779=ORIENTED_EDGE('',*,*,#3680,.T.);
#4780=ORIENTED_EDGE('',*,*,#3681,.T.);
#4781=ORIENTED_EDGE('',*,*,#3682,.F.);
#4782=ORIENTED_EDGE('',*,*,#3683,.T.);
#4783=ORIENTED_EDGE('',*,*,#3684,.T.);
#4784=ORIENTED_EDGE('',*,*,#3675,.T.);
#4785=ORIENTED_EDGE('',*,*,#3685,.T.);
#4786=ORIENTED_EDGE('',*,*,#3686,.T.);
#4787=ORIENTED_EDGE('',*,*,#3678,.T.);
#4788=ORIENTED_EDGE('',*,*,#3687,.F.);
#4789=ORIENTED_EDGE('',*,*,#3688,.T.);
#4790=ORIENTED_EDGE('',*,*,#3684,.F.);
#4791=ORIENTED_EDGE('',*,*,#3688,.F.);
#4792=ORIENTED_EDGE('',*,*,#3689,.F.);
#4793=ORIENTED_EDGE('',*,*,#3690,.T.);
#4794=ORIENTED_EDGE('',*,*,#3683,.F.);
#4795=ORIENTED_EDGE('',*,*,#3690,.F.);
#4796=ORIENTED_EDGE('',*,*,#3691,.F.);
#4797=ORIENTED_EDGE('',*,*,#3692,.T.);
#4798=ORIENTED_EDGE('',*,*,#3693,.F.);
#4799=ORIENTED_EDGE('',*,*,#3694,.F.);
#4800=ORIENTED_EDGE('',*,*,#3670,.T.);
#4801=ORIENTED_EDGE('',*,*,#3673,.T.);
#4802=ORIENTED_EDGE('',*,*,#3691,.T.);
#4803=ORIENTED_EDGE('',*,*,#3695,.T.);
#4804=ORIENTED_EDGE('',*,*,#3696,.T.);
#4805=ORIENTED_EDGE('',*,*,#3697,.T.);
#4806=ORIENTED_EDGE('',*,*,#3698,.T.);
#4807=ORIENTED_EDGE('',*,*,#3679,.T.);
#4808=ORIENTED_EDGE('',*,*,#3686,.F.);
#4809=ORIENTED_EDGE('',*,*,#3699,.F.);
#4810=ORIENTED_EDGE('',*,*,#3692,.F.);
#4811=ORIENTED_EDGE('',*,*,#3697,.F.);
#4812=ORIENTED_EDGE('',*,*,#3674,.T.);
#4813=ORIENTED_EDGE('',*,*,#3700,.F.);
#4814=ORIENTED_EDGE('',*,*,#3701,.F.);
#4815=ORIENTED_EDGE('',*,*,#3693,.T.);
#4816=ORIENTED_EDGE('',*,*,#3699,.T.);
#4817=ORIENTED_EDGE('',*,*,#3685,.F.);
#4818=ORIENTED_EDGE('',*,*,#3687,.T.);
#4819=ORIENTED_EDGE('',*,*,#3689,.T.);
#4820=ORIENTED_EDGE('',*,*,#3702,.T.);
#4821=ORIENTED_EDGE('',*,*,#3695,.F.);
#4822=ORIENTED_EDGE('',*,*,#3694,.T.);
#4823=ORIENTED_EDGE('',*,*,#3701,.T.);
#4824=ORIENTED_EDGE('',*,*,#3703,.F.);
#4825=ORIENTED_EDGE('',*,*,#3681,.F.);
#4826=ORIENTED_EDGE('',*,*,#3677,.T.);
#4827=ORIENTED_EDGE('',*,*,#3682,.T.);
#4828=ORIENTED_EDGE('',*,*,#3703,.T.);
#4829=ORIENTED_EDGE('',*,*,#3700,.T.);
#4830=ORIENTED_EDGE('',*,*,#3702,.F.);
#4831=ORIENTED_EDGE('',*,*,#3680,.F.);
#4832=ORIENTED_EDGE('',*,*,#3698,.F.);
#4833=ORIENTED_EDGE('',*,*,#3696,.F.);
#4834=ORIENTED_EDGE('',*,*,#3668,.T.);
#4835=ORIENTED_EDGE('',*,*,#3671,.T.);
#4836=ORIENTED_EDGE('',*,*,#3704,.T.);
#4837=ORIENTED_EDGE('',*,*,#3705,.T.);
#4838=ORIENTED_EDGE('',*,*,#3706,.T.);
#4839=ORIENTED_EDGE('',*,*,#3707,.F.);
#4840=ORIENTED_EDGE('',*,*,#3708,.T.);
#4841=ORIENTED_EDGE('',*,*,#3709,.T.);
#4842=ORIENTED_EDGE('',*,*,#3710,.T.);
#4843=ORIENTED_EDGE('',*,*,#3705,.F.);
#4844=ORIENTED_EDGE('',*,*,#3711,.T.);
#4845=ORIENTED_EDGE('',*,*,#3712,.T.);
#4846=ORIENTED_EDGE('',*,*,#3713,.T.);
#4847=ORIENTED_EDGE('',*,*,#3709,.F.);
#4848=ORIENTED_EDGE('',*,*,#3714,.T.);
#4849=ORIENTED_EDGE('',*,*,#3715,.T.);
#4850=ORIENTED_EDGE('',*,*,#3716,.T.);
#4851=ORIENTED_EDGE('',*,*,#3712,.F.);
#4852=ORIENTED_EDGE('',*,*,#3717,.T.);
#4853=ORIENTED_EDGE('',*,*,#3718,.T.);
#4854=ORIENTED_EDGE('',*,*,#3719,.T.);
#4855=ORIENTED_EDGE('',*,*,#3715,.F.);
#4856=ORIENTED_EDGE('',*,*,#3720,.T.);
#4857=ORIENTED_EDGE('',*,*,#3707,.T.);
#4858=ORIENTED_EDGE('',*,*,#3721,.T.);
#4859=ORIENTED_EDGE('',*,*,#3718,.F.);
#4860=ORIENTED_EDGE('',*,*,#3720,.F.);
#4861=ORIENTED_EDGE('',*,*,#3717,.F.);
#4862=ORIENTED_EDGE('',*,*,#3714,.F.);
#4863=ORIENTED_EDGE('',*,*,#3711,.F.);
#4864=ORIENTED_EDGE('',*,*,#3708,.F.);
#4865=ORIENTED_EDGE('',*,*,#3704,.F.);
#4866=ORIENTED_EDGE('',*,*,#3721,.F.);
#4867=ORIENTED_EDGE('',*,*,#3706,.F.);
#4868=ORIENTED_EDGE('',*,*,#3710,.F.);
#4869=ORIENTED_EDGE('',*,*,#3713,.F.);
#4870=ORIENTED_EDGE('',*,*,#3716,.F.);
#4871=ORIENTED_EDGE('',*,*,#3719,.F.);
#4872=ORIENTED_EDGE('',*,*,#3722,.F.);
#4873=ORIENTED_EDGE('',*,*,#3723,.F.);
#4874=ORIENTED_EDGE('',*,*,#3724,.F.);
#4875=ORIENTED_EDGE('',*,*,#3725,.T.);
#4876=ORIENTED_EDGE('',*,*,#3723,.T.);
#4877=ORIENTED_EDGE('',*,*,#3725,.F.);
#4878=ORIENTED_EDGE('',*,*,#3726,.F.);
#4879=ORIENTED_EDGE('',*,*,#3727,.T.);
#4880=ORIENTED_EDGE('',*,*,#3724,.T.);
#4881=ORIENTED_EDGE('',*,*,#3727,.F.);
#4882=ORIENTED_EDGE('',*,*,#3728,.F.);
#4883=ORIENTED_EDGE('',*,*,#3729,.T.);
#4884=ORIENTED_EDGE('',*,*,#3726,.T.);
#4885=ORIENTED_EDGE('',*,*,#3729,.F.);
#4886=ORIENTED_EDGE('',*,*,#3728,.T.);
#4887=ORIENTED_EDGE('',*,*,#3730,.F.);
#4888=ORIENTED_EDGE('',*,*,#3731,.F.);
#4889=ORIENTED_EDGE('',*,*,#3732,.T.);
#4890=ORIENTED_EDGE('',*,*,#3730,.T.);
#4891=ORIENTED_EDGE('',*,*,#3732,.F.);
#4892=ORIENTED_EDGE('',*,*,#3722,.T.);
#4893=ORIENTED_EDGE('',*,*,#3733,.T.);
#4894=ORIENTED_EDGE('',*,*,#3731,.T.);
#4895=ORIENTED_EDGE('',*,*,#3733,.F.);
#4896=ORIENTED_EDGE('',*,*,#3734,.F.);
#4897=ORIENTED_EDGE('',*,*,#3735,.T.);
#4898=ORIENTED_EDGE('',*,*,#3736,.F.);
#4899=ORIENTED_EDGE('',*,*,#3735,.F.);
#4900=ORIENTED_EDGE('',*,*,#3734,.T.);
#4901=ORIENTED_EDGE('',*,*,#3737,.T.);
#4902=ORIENTED_EDGE('',*,*,#3738,.F.);
#4903=ORIENTED_EDGE('',*,*,#3737,.F.);
#4904=ORIENTED_EDGE('',*,*,#3739,.T.);
#4905=ORIENTED_EDGE('',*,*,#3740,.T.);
#4906=ORIENTED_EDGE('',*,*,#3739,.F.);
#4907=ORIENTED_EDGE('',*,*,#3740,.F.);
#4908=ORIENTED_EDGE('',*,*,#3741,.F.);
#4909=ORIENTED_EDGE('',*,*,#3742,.T.);
#4910=ORIENTED_EDGE('',*,*,#3738,.T.);
#4911=ORIENTED_EDGE('',*,*,#3742,.F.);
#4912=ORIENTED_EDGE('',*,*,#3741,.T.);
#4913=ORIENTED_EDGE('',*,*,#3736,.T.);
#4914=ORIENTED_EDGE('',*,*,#3743,.F.);
#4915=ORIENTED_EDGE('',*,*,#3744,.T.);
#4916=ORIENTED_EDGE('',*,*,#3745,.T.);
#4917=ORIENTED_EDGE('',*,*,#3744,.F.);
#4918=ORIENTED_EDGE('',*,*,#3746,.F.);
#4919=ORIENTED_EDGE('',*,*,#3747,.T.);
#4920=ORIENTED_EDGE('',*,*,#3748,.T.);
#4921=ORIENTED_EDGE('',*,*,#3747,.F.);
#4922=ORIENTED_EDGE('',*,*,#3746,.T.);
#4923=ORIENTED_EDGE('',*,*,#3743,.T.);
#4924=ORIENTED_EDGE('',*,*,#3748,.F.);
#4925=ORIENTED_EDGE('',*,*,#3745,.F.);
#4926=ORIENTED_EDGE('',*,*,#3749,.F.);
#4927=ORIENTED_EDGE('',*,*,#3750,.T.);
#4928=ORIENTED_EDGE('',*,*,#3751,.T.);
#4929=ORIENTED_EDGE('',*,*,#3750,.F.);
#4930=ORIENTED_EDGE('',*,*,#3752,.F.);
#4931=ORIENTED_EDGE('',*,*,#3753,.T.);
#4932=ORIENTED_EDGE('',*,*,#3754,.T.);
#4933=ORIENTED_EDGE('',*,*,#3753,.F.);
#4934=ORIENTED_EDGE('',*,*,#3752,.T.);
#4935=ORIENTED_EDGE('',*,*,#3749,.T.);
#4936=ORIENTED_EDGE('',*,*,#3754,.F.);
#4937=ORIENTED_EDGE('',*,*,#3751,.F.);
#4938=ORIENTED_EDGE('',*,*,#3755,.F.);
#4939=ORIENTED_EDGE('',*,*,#3756,.T.);
#4940=ORIENTED_EDGE('',*,*,#3757,.F.);
#4941=ORIENTED_EDGE('',*,*,#3756,.F.);
#4942=ORIENTED_EDGE('',*,*,#3755,.T.);
#4943=ORIENTED_EDGE('',*,*,#3758,.T.);
#4944=ORIENTED_EDGE('',*,*,#3759,.F.);
#4945=ORIENTED_EDGE('',*,*,#3758,.F.);
#4946=ORIENTED_EDGE('',*,*,#3760,.T.);
#4947=ORIENTED_EDGE('',*,*,#3761,.T.);
#4948=ORIENTED_EDGE('',*,*,#3760,.F.);
#4949=ORIENTED_EDGE('',*,*,#3761,.F.);
#4950=ORIENTED_EDGE('',*,*,#3762,.F.);
#4951=ORIENTED_EDGE('',*,*,#3763,.T.);
#4952=ORIENTED_EDGE('',*,*,#3759,.T.);
#4953=ORIENTED_EDGE('',*,*,#3763,.F.);
#4954=ORIENTED_EDGE('',*,*,#3762,.T.);
#4955=ORIENTED_EDGE('',*,*,#3757,.T.);
#4956=ORIENTED_EDGE('',*,*,#3764,.F.);
#4957=ORIENTED_EDGE('',*,*,#3765,.T.);
#4958=ORIENTED_EDGE('',*,*,#3766,.T.);
#4959=ORIENTED_EDGE('',*,*,#3765,.F.);
#4960=ORIENTED_EDGE('',*,*,#3767,.F.);
#4961=ORIENTED_EDGE('',*,*,#3768,.T.);
#4962=ORIENTED_EDGE('',*,*,#3769,.T.);
#4963=ORIENTED_EDGE('',*,*,#3768,.F.);
#4964=ORIENTED_EDGE('',*,*,#3767,.T.);
#4965=ORIENTED_EDGE('',*,*,#3764,.T.);
#4966=ORIENTED_EDGE('',*,*,#3769,.F.);
#4967=ORIENTED_EDGE('',*,*,#3766,.F.);
#4968=ORIENTED_EDGE('',*,*,#3770,.F.);
#4969=ORIENTED_EDGE('',*,*,#3771,.T.);
#4970=ORIENTED_EDGE('',*,*,#3772,.T.);
#4971=ORIENTED_EDGE('',*,*,#3771,.F.);
#4972=ORIENTED_EDGE('',*,*,#3773,.F.);
#4973=ORIENTED_EDGE('',*,*,#3774,.T.);
#4974=ORIENTED_EDGE('',*,*,#3775,.T.);
#4975=ORIENTED_EDGE('',*,*,#3774,.F.);
#4976=ORIENTED_EDGE('',*,*,#3773,.T.);
#4977=ORIENTED_EDGE('',*,*,#3770,.T.);
#4978=ORIENTED_EDGE('',*,*,#3775,.F.);
#4979=ORIENTED_EDGE('',*,*,#3772,.F.);
#4980=ORIENTED_EDGE('',*,*,#3776,.T.);
#4981=ORIENTED_EDGE('',*,*,#3777,.T.);
#4982=ORIENTED_EDGE('',*,*,#3778,.T.);
#4983=ORIENTED_EDGE('',*,*,#3779,.F.);
#4984=ORIENTED_EDGE('',*,*,#3780,.T.);
#4985=ORIENTED_EDGE('',*,*,#3781,.T.);
#4986=ORIENTED_EDGE('',*,*,#3782,.T.);
#4987=ORIENTED_EDGE('',*,*,#3777,.F.);
#4988=ORIENTED_EDGE('',*,*,#3783,.T.);
#4989=ORIENTED_EDGE('',*,*,#3784,.T.);
#4990=ORIENTED_EDGE('',*,*,#3785,.T.);
#4991=ORIENTED_EDGE('',*,*,#3781,.F.);
#4992=ORIENTED_EDGE('',*,*,#3786,.T.);
#4993=ORIENTED_EDGE('',*,*,#3787,.T.);
#4994=ORIENTED_EDGE('',*,*,#3788,.T.);
#4995=ORIENTED_EDGE('',*,*,#3784,.F.);
#4996=ORIENTED_EDGE('',*,*,#3789,.T.);
#4997=ORIENTED_EDGE('',*,*,#3790,.T.);
#4998=ORIENTED_EDGE('',*,*,#3791,.T.);
#4999=ORIENTED_EDGE('',*,*,#3787,.F.);
#5000=ORIENTED_EDGE('',*,*,#3792,.T.);
#5001=ORIENTED_EDGE('',*,*,#3779,.T.);
#5002=ORIENTED_EDGE('',*,*,#3793,.T.);
#5003=ORIENTED_EDGE('',*,*,#3790,.F.);
#5004=ORIENTED_EDGE('',*,*,#3792,.F.);
#5005=ORIENTED_EDGE('',*,*,#3789,.F.);
#5006=ORIENTED_EDGE('',*,*,#3786,.F.);
#5007=ORIENTED_EDGE('',*,*,#3783,.F.);
#5008=ORIENTED_EDGE('',*,*,#3780,.F.);
#5009=ORIENTED_EDGE('',*,*,#3776,.F.);
#5010=ORIENTED_EDGE('',*,*,#3793,.F.);
#5011=ORIENTED_EDGE('',*,*,#3778,.F.);
#5012=ORIENTED_EDGE('',*,*,#3782,.F.);
#5013=ORIENTED_EDGE('',*,*,#3785,.F.);
#5014=ORIENTED_EDGE('',*,*,#3788,.F.);
#5015=ORIENTED_EDGE('',*,*,#3791,.F.);
#5016=ORIENTED_EDGE('',*,*,#3794,.F.);
#5017=ORIENTED_EDGE('',*,*,#3795,.F.);
#5018=ORIENTED_EDGE('',*,*,#3796,.F.);
#5019=ORIENTED_EDGE('',*,*,#3797,.T.);
#5020=ORIENTED_EDGE('',*,*,#3795,.T.);
#5021=ORIENTED_EDGE('',*,*,#3797,.F.);
#5022=ORIENTED_EDGE('',*,*,#3798,.F.);
#5023=ORIENTED_EDGE('',*,*,#3799,.T.);
#5024=ORIENTED_EDGE('',*,*,#3796,.T.);
#5025=ORIENTED_EDGE('',*,*,#3799,.F.);
#5026=ORIENTED_EDGE('',*,*,#3800,.F.);
#5027=ORIENTED_EDGE('',*,*,#3801,.T.);
#5028=ORIENTED_EDGE('',*,*,#3798,.T.);
#5029=ORIENTED_EDGE('',*,*,#3801,.F.);
#5030=ORIENTED_EDGE('',*,*,#3800,.T.);
#5031=ORIENTED_EDGE('',*,*,#3802,.F.);
#5032=ORIENTED_EDGE('',*,*,#3803,.F.);
#5033=ORIENTED_EDGE('',*,*,#3804,.T.);
#5034=ORIENTED_EDGE('',*,*,#3802,.T.);
#5035=ORIENTED_EDGE('',*,*,#3804,.F.);
#5036=ORIENTED_EDGE('',*,*,#3794,.T.);
#5037=ORIENTED_EDGE('',*,*,#3805,.T.);
#5038=ORIENTED_EDGE('',*,*,#3803,.T.);
#5039=ORIENTED_EDGE('',*,*,#3805,.F.);
#5040=ORIENTED_EDGE('',*,*,#3806,.F.);
#5041=ORIENTED_EDGE('',*,*,#3807,.T.);
#5042=ORIENTED_EDGE('',*,*,#3808,.F.);
#5043=ORIENTED_EDGE('',*,*,#3807,.F.);
#5044=ORIENTED_EDGE('',*,*,#3806,.T.);
#5045=ORIENTED_EDGE('',*,*,#3809,.F.);
#5046=ORIENTED_EDGE('',*,*,#3810,.T.);
#5047=ORIENTED_EDGE('',*,*,#3811,.F.);
#5048=ORIENTED_EDGE('',*,*,#3810,.F.);
#5049=ORIENTED_EDGE('',*,*,#3812,.F.);
#5050=ORIENTED_EDGE('',*,*,#3813,.T.);
#5051=ORIENTED_EDGE('',*,*,#3814,.F.);
#5052=ORIENTED_EDGE('',*,*,#3813,.F.);
#5053=ORIENTED_EDGE('',*,*,#3815,.T.);
#5054=ORIENTED_EDGE('',*,*,#3816,.T.);
#5055=ORIENTED_EDGE('',*,*,#3817,.F.);
#5056=ORIENTED_EDGE('',*,*,#3818,.F.);
#5057=ORIENTED_EDGE('',*,*,#3819,.T.);
#5058=ORIENTED_EDGE('',*,*,#3818,.T.);
#5059=ORIENTED_EDGE('',*,*,#3820,.F.);
#5060=ORIENTED_EDGE('',*,*,#3821,.F.);
#5061=ORIENTED_EDGE('',*,*,#3822,.T.);
#5062=ORIENTED_EDGE('',*,*,#3821,.T.);
#5063=ORIENTED_EDGE('',*,*,#3823,.F.);
#5064=ORIENTED_EDGE('',*,*,#3824,.F.);
#5065=ORIENTED_EDGE('',*,*,#3825,.T.);
#5066=ORIENTED_EDGE('',*,*,#3824,.T.);
#5067=ORIENTED_EDGE('',*,*,#3826,.F.);
#5068=ORIENTED_EDGE('',*,*,#3816,.F.);
#5069=ORIENTED_EDGE('',*,*,#3826,.T.);
#5070=ORIENTED_EDGE('',*,*,#3823,.T.);
#5071=ORIENTED_EDGE('',*,*,#3820,.T.);
#5072=ORIENTED_EDGE('',*,*,#3817,.T.);
#5073=ORIENTED_EDGE('',*,*,#3808,.T.);
#5074=ORIENTED_EDGE('',*,*,#3811,.T.);
#5075=ORIENTED_EDGE('',*,*,#3814,.T.);
#5076=ORIENTED_EDGE('',*,*,#3825,.F.);
#5077=ORIENTED_EDGE('',*,*,#3815,.F.);
#5078=ORIENTED_EDGE('',*,*,#3819,.F.);
#5079=ORIENTED_EDGE('',*,*,#3822,.F.);
#5080=ORIENTED_EDGE('',*,*,#3809,.T.);
#5081=ORIENTED_EDGE('',*,*,#3812,.T.);
#5082=ORIENTED_EDGE('',*,*,#3827,.T.);
#5083=ORIENTED_EDGE('',*,*,#3828,.T.);
#5084=ORIENTED_EDGE('',*,*,#3829,.T.);
#5085=ORIENTED_EDGE('',*,*,#3830,.F.);
#5086=ORIENTED_EDGE('',*,*,#3831,.T.);
#5087=ORIENTED_EDGE('',*,*,#3832,.T.);
#5088=ORIENTED_EDGE('',*,*,#3833,.T.);
#5089=ORIENTED_EDGE('',*,*,#3828,.F.);
#5090=ORIENTED_EDGE('',*,*,#3834,.T.);
#5091=ORIENTED_EDGE('',*,*,#3835,.T.);
#5092=ORIENTED_EDGE('',*,*,#3836,.T.);
#5093=ORIENTED_EDGE('',*,*,#3832,.F.);
#5094=ORIENTED_EDGE('',*,*,#3837,.T.);
#5095=ORIENTED_EDGE('',*,*,#3838,.T.);
#5096=ORIENTED_EDGE('',*,*,#3839,.T.);
#5097=ORIENTED_EDGE('',*,*,#3835,.F.);
#5098=ORIENTED_EDGE('',*,*,#3840,.T.);
#5099=ORIENTED_EDGE('',*,*,#3841,.T.);
#5100=ORIENTED_EDGE('',*,*,#3842,.T.);
#5101=ORIENTED_EDGE('',*,*,#3838,.F.);
#5102=ORIENTED_EDGE('',*,*,#3843,.T.);
#5103=ORIENTED_EDGE('',*,*,#3830,.T.);
#5104=ORIENTED_EDGE('',*,*,#3844,.T.);
#5105=ORIENTED_EDGE('',*,*,#3841,.F.);
#5106=ORIENTED_EDGE('',*,*,#3843,.F.);
#5107=ORIENTED_EDGE('',*,*,#3840,.F.);
#5108=ORIENTED_EDGE('',*,*,#3837,.F.);
#5109=ORIENTED_EDGE('',*,*,#3834,.F.);
#5110=ORIENTED_EDGE('',*,*,#3831,.F.);
#5111=ORIENTED_EDGE('',*,*,#3827,.F.);
#5112=ORIENTED_EDGE('',*,*,#3844,.F.);
#5113=ORIENTED_EDGE('',*,*,#3829,.F.);
#5114=ORIENTED_EDGE('',*,*,#3833,.F.);
#5115=ORIENTED_EDGE('',*,*,#3836,.F.);
#5116=ORIENTED_EDGE('',*,*,#3839,.F.);
#5117=ORIENTED_EDGE('',*,*,#3842,.F.);
#5118=ORIENTED_EDGE('',*,*,#3845,.F.);
#5119=ORIENTED_EDGE('',*,*,#3846,.F.);
#5120=ORIENTED_EDGE('',*,*,#3847,.F.);
#5121=ORIENTED_EDGE('',*,*,#3848,.T.);
#5122=ORIENTED_EDGE('',*,*,#3846,.T.);
#5123=ORIENTED_EDGE('',*,*,#3848,.F.);
#5124=ORIENTED_EDGE('',*,*,#3849,.F.);
#5125=ORIENTED_EDGE('',*,*,#3850,.T.);
#5126=ORIENTED_EDGE('',*,*,#3847,.T.);
#5127=ORIENTED_EDGE('',*,*,#3850,.F.);
#5128=ORIENTED_EDGE('',*,*,#3851,.F.);
#5129=ORIENTED_EDGE('',*,*,#3852,.T.);
#5130=ORIENTED_EDGE('',*,*,#3849,.T.);
#5131=ORIENTED_EDGE('',*,*,#3852,.F.);
#5132=ORIENTED_EDGE('',*,*,#3851,.T.);
#5133=ORIENTED_EDGE('',*,*,#3853,.F.);
#5134=ORIENTED_EDGE('',*,*,#3854,.F.);
#5135=ORIENTED_EDGE('',*,*,#3855,.T.);
#5136=ORIENTED_EDGE('',*,*,#3853,.T.);
#5137=ORIENTED_EDGE('',*,*,#3855,.F.);
#5138=ORIENTED_EDGE('',*,*,#3845,.T.);
#5139=ORIENTED_EDGE('',*,*,#3856,.T.);
#5140=ORIENTED_EDGE('',*,*,#3854,.T.);
#5141=ORIENTED_EDGE('',*,*,#3856,.F.);
#5142=ORIENTED_EDGE('',*,*,#3857,.F.);
#5143=ORIENTED_EDGE('',*,*,#3858,.T.);
#5144=ORIENTED_EDGE('',*,*,#3859,.T.);
#5145=ORIENTED_EDGE('',*,*,#3860,.F.);
#5146=ORIENTED_EDGE('',*,*,#3861,.F.);
#5147=ORIENTED_EDGE('',*,*,#3862,.F.);
#5148=ORIENTED_EDGE('',*,*,#3859,.F.);
#5149=ORIENTED_EDGE('',*,*,#3863,.T.);
#5150=ORIENTED_EDGE('',*,*,#3864,.F.);
#5151=ORIENTED_EDGE('',*,*,#3863,.F.);
#5152=ORIENTED_EDGE('',*,*,#3858,.F.);
#5153=ORIENTED_EDGE('',*,*,#3865,.F.);
#5154=ORIENTED_EDGE('',*,*,#3861,.T.);
#5155=ORIENTED_EDGE('',*,*,#3866,.F.);
#5156=ORIENTED_EDGE('',*,*,#3867,.T.);
#5157=ORIENTED_EDGE('',*,*,#3868,.T.);
#5158=ORIENTED_EDGE('',*,*,#3869,.F.);
#5159=ORIENTED_EDGE('',*,*,#3870,.F.);
#5160=ORIENTED_EDGE('',*,*,#3871,.F.);
#5161=ORIENTED_EDGE('',*,*,#3868,.F.);
#5162=ORIENTED_EDGE('',*,*,#3872,.T.);
#5163=ORIENTED_EDGE('',*,*,#3873,.F.);
#5164=ORIENTED_EDGE('',*,*,#3872,.F.);
#5165=ORIENTED_EDGE('',*,*,#3867,.F.);
#5166=ORIENTED_EDGE('',*,*,#3874,.F.);
#5167=ORIENTED_EDGE('',*,*,#3870,.T.);
#5168=ORIENTED_EDGE('',*,*,#3875,.F.);
#5169=ORIENTED_EDGE('',*,*,#3876,.T.);
#5170=ORIENTED_EDGE('',*,*,#3877,.F.);
#5171=ORIENTED_EDGE('',*,*,#3876,.F.);
#5172=ORIENTED_EDGE('',*,*,#3862,.T.);
#5173=ORIENTED_EDGE('',*,*,#3865,.T.);
#5174=ORIENTED_EDGE('',*,*,#3860,.T.);
#5175=ORIENTED_EDGE('',*,*,#3857,.T.);
#5176=ORIENTED_EDGE('',*,*,#3878,.F.);
#5177=ORIENTED_EDGE('',*,*,#3879,.T.);
#5178=ORIENTED_EDGE('',*,*,#3880,.F.);
#5179=ORIENTED_EDGE('',*,*,#3879,.F.);
#5180=ORIENTED_EDGE('',*,*,#3871,.T.);
#5181=ORIENTED_EDGE('',*,*,#3874,.T.);
#5182=ORIENTED_EDGE('',*,*,#3869,.T.);
#5183=ORIENTED_EDGE('',*,*,#3866,.T.);
#5184=ORIENTED_EDGE('',*,*,#3881,.T.);
#5185=ORIENTED_EDGE('',*,*,#3882,.T.);
#5186=ORIENTED_EDGE('',*,*,#3883,.F.);
#5187=ORIENTED_EDGE('',*,*,#3884,.F.);
#5188=ORIENTED_EDGE('',*,*,#3864,.T.);
#5189=ORIENTED_EDGE('',*,*,#3873,.T.);
#5190=ORIENTED_EDGE('',*,*,#3885,.T.);
#5191=ORIENTED_EDGE('',*,*,#3884,.T.);
#5192=ORIENTED_EDGE('',*,*,#3886,.F.);
#5193=ORIENTED_EDGE('',*,*,#3887,.F.);
#5194=ORIENTED_EDGE('',*,*,#3888,.T.);
#5195=ORIENTED_EDGE('',*,*,#3887,.T.);
#5196=ORIENTED_EDGE('',*,*,#3889,.F.);
#5197=ORIENTED_EDGE('',*,*,#3890,.F.);
#5198=ORIENTED_EDGE('',*,*,#3891,.T.);
#5199=ORIENTED_EDGE('',*,*,#3890,.T.);
#5200=ORIENTED_EDGE('',*,*,#3892,.F.);
#5201=ORIENTED_EDGE('',*,*,#3882,.F.);
#5202=ORIENTED_EDGE('',*,*,#3892,.T.);
#5203=ORIENTED_EDGE('',*,*,#3889,.T.);
#5204=ORIENTED_EDGE('',*,*,#3886,.T.);
#5205=ORIENTED_EDGE('',*,*,#3883,.T.);
#5206=ORIENTED_EDGE('',*,*,#3877,.T.);
#5207=ORIENTED_EDGE('',*,*,#3880,.T.);
#5208=ORIENTED_EDGE('',*,*,#3891,.F.);
#5209=ORIENTED_EDGE('',*,*,#3881,.F.);
#5210=ORIENTED_EDGE('',*,*,#3885,.F.);
#5211=ORIENTED_EDGE('',*,*,#3888,.F.);
#5212=ORIENTED_EDGE('',*,*,#3875,.T.);
#5213=ORIENTED_EDGE('',*,*,#3878,.T.);
#5214=ORIENTED_EDGE('',*,*,#3893,.F.);
#5215=ORIENTED_EDGE('',*,*,#3894,.T.);
#5216=ORIENTED_EDGE('',*,*,#3895,.T.);
#5217=ORIENTED_EDGE('',*,*,#3896,.F.);
#5218=ORIENTED_EDGE('',*,*,#3897,.F.);
#5219=ORIENTED_EDGE('',*,*,#3898,.T.);
#5220=ORIENTED_EDGE('',*,*,#3899,.T.);
#5221=ORIENTED_EDGE('',*,*,#3894,.F.);
#5222=ORIENTED_EDGE('',*,*,#3900,.F.);
#5223=ORIENTED_EDGE('',*,*,#3901,.T.);
#5224=ORIENTED_EDGE('',*,*,#3902,.T.);
#5225=ORIENTED_EDGE('',*,*,#3898,.F.);
#5226=ORIENTED_EDGE('',*,*,#3903,.F.);
#5227=ORIENTED_EDGE('',*,*,#3904,.T.);
#5228=ORIENTED_EDGE('',*,*,#3905,.T.);
#5229=ORIENTED_EDGE('',*,*,#3901,.F.);
#5230=ORIENTED_EDGE('',*,*,#3906,.F.);
#5231=ORIENTED_EDGE('',*,*,#3907,.T.);
#5232=ORIENTED_EDGE('',*,*,#3908,.T.);
#5233=ORIENTED_EDGE('',*,*,#3904,.F.);
#5234=ORIENTED_EDGE('',*,*,#3909,.F.);
#5235=ORIENTED_EDGE('',*,*,#3896,.T.);
#5236=ORIENTED_EDGE('',*,*,#3910,.T.);
#5237=ORIENTED_EDGE('',*,*,#3907,.F.);
#5238=ORIENTED_EDGE('',*,*,#3910,.F.);
#5239=ORIENTED_EDGE('',*,*,#3895,.F.);
#5240=ORIENTED_EDGE('',*,*,#3899,.F.);
#5241=ORIENTED_EDGE('',*,*,#3902,.F.);
#5242=ORIENTED_EDGE('',*,*,#3905,.F.);
#5243=ORIENTED_EDGE('',*,*,#3908,.F.);
#5244=ORIENTED_EDGE('',*,*,#3911,.F.);
#5245=ORIENTED_EDGE('',*,*,#3893,.T.);
#5246=ORIENTED_EDGE('',*,*,#3909,.T.);
#5247=ORIENTED_EDGE('',*,*,#3906,.T.);
#5248=ORIENTED_EDGE('',*,*,#3903,.T.);
#5249=ORIENTED_EDGE('',*,*,#3900,.T.);
#5250=ORIENTED_EDGE('',*,*,#3897,.T.);
#5251=ORIENTED_EDGE('',*,*,#3912,.F.);
#5252=ORIENTED_EDGE('',*,*,#3913,.T.);
#5253=ORIENTED_EDGE('',*,*,#3911,.T.);
#5254=ORIENTED_EDGE('',*,*,#3913,.F.);
#5255=ORIENTED_EDGE('',*,*,#3914,.F.);
#5256=ORIENTED_EDGE('',*,*,#3915,.T.);
#5257=ORIENTED_EDGE('',*,*,#3912,.T.);
#5258=ORIENTED_EDGE('',*,*,#3915,.F.);
#5259=ORIENTED_EDGE('',*,*,#3916,.F.);
#5260=ORIENTED_EDGE('',*,*,#3917,.T.);
#5261=ORIENTED_EDGE('',*,*,#3914,.T.);
#5262=ORIENTED_EDGE('',*,*,#3917,.F.);
#5263=ORIENTED_EDGE('',*,*,#3916,.T.);
#5264=ORIENTED_EDGE('',*,*,#3918,.F.);
#5265=ORIENTED_EDGE('',*,*,#3919,.T.);
#5266=ORIENTED_EDGE('',*,*,#3920,.T.);
#5267=ORIENTED_EDGE('',*,*,#3919,.F.);
#5268=ORIENTED_EDGE('',*,*,#3920,.F.);
#5269=ORIENTED_EDGE('',*,*,#3921,.F.);
#5270=ORIENTED_EDGE('',*,*,#3922,.F.);
#5271=ORIENTED_EDGE('',*,*,#3923,.T.);
#5272=ORIENTED_EDGE('',*,*,#3924,.T.);
#5273=ORIENTED_EDGE('',*,*,#3923,.F.);
#5274=ORIENTED_EDGE('',*,*,#3924,.F.);
#5275=ORIENTED_EDGE('',*,*,#3918,.T.);
#5276=ORIENTED_EDGE('',*,*,#3925,.F.);
#5277=ORIENTED_EDGE('',*,*,#3926,.T.);
#5278=ORIENTED_EDGE('',*,*,#3927,.T.);
#5279=ORIENTED_EDGE('',*,*,#3926,.F.);
#5280=ORIENTED_EDGE('',*,*,#3921,.T.);
#5281=ORIENTED_EDGE('',*,*,#3922,.T.);
#5282=ORIENTED_EDGE('',*,*,#3925,.T.);
#5283=ORIENTED_EDGE('',*,*,#3927,.F.);
#5284=ORIENTED_EDGE('',*,*,#3928,.F.);
#5285=ORIENTED_EDGE('',*,*,#3929,.T.);
#5286=ORIENTED_EDGE('',*,*,#3930,.T.);
#5287=ORIENTED_EDGE('',*,*,#3929,.F.);
#5288=ORIENTED_EDGE('',*,*,#3928,.T.);
#5289=ORIENTED_EDGE('',*,*,#3930,.F.);
#5290=ORIENTED_EDGE('',*,*,#3931,.F.);
#5291=ORIENTED_EDGE('',*,*,#3932,.T.);
#5292=ORIENTED_EDGE('',*,*,#3933,.F.);
#5293=ORIENTED_EDGE('',*,*,#3934,.F.);
#5294=ORIENTED_EDGE('',*,*,#3935,.F.);
#5295=ORIENTED_EDGE('',*,*,#3934,.T.);
#5296=ORIENTED_EDGE('',*,*,#3936,.F.);
#5297=ORIENTED_EDGE('',*,*,#3937,.F.);
#5298=ORIENTED_EDGE('',*,*,#3938,.F.);
#5299=ORIENTED_EDGE('',*,*,#3937,.T.);
#5300=ORIENTED_EDGE('',*,*,#3939,.F.);
#5301=ORIENTED_EDGE('',*,*,#3932,.F.);
#5302=ORIENTED_EDGE('',*,*,#3939,.T.);
#5303=ORIENTED_EDGE('',*,*,#3936,.T.);
#5304=ORIENTED_EDGE('',*,*,#3933,.T.);
#5305=ORIENTED_EDGE('',*,*,#3938,.T.);
#5306=ORIENTED_EDGE('',*,*,#3931,.T.);
#5307=ORIENTED_EDGE('',*,*,#3935,.T.);
#5308=ORIENTED_EDGE('',*,*,#3940,.F.);
#5309=ORIENTED_EDGE('',*,*,#3941,.T.);
#5310=ORIENTED_EDGE('',*,*,#3942,.T.);
#5311=ORIENTED_EDGE('',*,*,#3941,.F.);
#5312=ORIENTED_EDGE('',*,*,#3940,.T.);
#5313=ORIENTED_EDGE('',*,*,#3942,.F.);
#5314=ORIENTED_EDGE('',*,*,#3943,.F.);
#5315=ORIENTED_EDGE('',*,*,#3944,.T.);
#5316=ORIENTED_EDGE('',*,*,#3945,.T.);
#5317=ORIENTED_EDGE('',*,*,#3944,.F.);
#5318=ORIENTED_EDGE('',*,*,#3946,.F.);
#5319=ORIENTED_EDGE('',*,*,#3947,.T.);
#5320=ORIENTED_EDGE('',*,*,#3948,.T.);
#5321=ORIENTED_EDGE('',*,*,#3947,.F.);
#5322=ORIENTED_EDGE('',*,*,#3946,.T.);
#5323=ORIENTED_EDGE('',*,*,#3943,.T.);
#5324=ORIENTED_EDGE('',*,*,#3948,.F.);
#5325=ORIENTED_EDGE('',*,*,#3945,.F.);
#5326=ORIENTED_EDGE('',*,*,#3949,.F.);
#5327=ORIENTED_EDGE('',*,*,#3950,.T.);
#5328=ORIENTED_EDGE('',*,*,#3951,.T.);
#5329=ORIENTED_EDGE('',*,*,#3950,.F.);
#5330=ORIENTED_EDGE('',*,*,#3952,.F.);
#5331=ORIENTED_EDGE('',*,*,#3953,.T.);
#5332=ORIENTED_EDGE('',*,*,#3954,.T.);
#5333=ORIENTED_EDGE('',*,*,#3953,.F.);
#5334=ORIENTED_EDGE('',*,*,#3952,.T.);
#5335=ORIENTED_EDGE('',*,*,#3949,.T.);
#5336=ORIENTED_EDGE('',*,*,#3954,.F.);
#5337=ORIENTED_EDGE('',*,*,#3951,.F.);
#5338=ORIENTED_EDGE('',*,*,#3955,.F.);
#5339=ORIENTED_EDGE('',*,*,#3956,.T.);
#5340=ORIENTED_EDGE('',*,*,#3957,.T.);
#5341=ORIENTED_EDGE('',*,*,#3956,.F.);
#5342=ORIENTED_EDGE('',*,*,#3958,.F.);
#5343=ORIENTED_EDGE('',*,*,#3959,.T.);
#5344=ORIENTED_EDGE('',*,*,#3960,.T.);
#5345=ORIENTED_EDGE('',*,*,#3959,.F.);
#5346=ORIENTED_EDGE('',*,*,#3958,.T.);
#5347=ORIENTED_EDGE('',*,*,#3955,.T.);
#5348=ORIENTED_EDGE('',*,*,#3960,.F.);
#5349=ORIENTED_EDGE('',*,*,#3957,.F.);
#5350=ORIENTED_EDGE('',*,*,#3961,.F.);
#5351=ORIENTED_EDGE('',*,*,#3962,.T.);
#5352=ORIENTED_EDGE('',*,*,#3963,.T.);
#5353=ORIENTED_EDGE('',*,*,#3962,.F.);
#5354=ORIENTED_EDGE('',*,*,#3961,.T.);
#5355=ORIENTED_EDGE('',*,*,#3963,.F.);
#5356=ORIENTED_EDGE('',*,*,#3964,.F.);
#5357=ORIENTED_EDGE('',*,*,#3965,.F.);
#5358=ORIENTED_EDGE('',*,*,#3966,.T.);
#5359=ORIENTED_EDGE('',*,*,#3967,.F.);
#5360=ORIENTED_EDGE('',*,*,#3968,.F.);
#5361=ORIENTED_EDGE('',*,*,#3966,.F.);
#5362=ORIENTED_EDGE('',*,*,#3967,.T.);
#5363=ORIENTED_EDGE('',*,*,#3968,.T.);
#5364=ORIENTED_EDGE('',*,*,#3969,.T.);
#5365=ORIENTED_EDGE('',*,*,#3970,.T.);
#5366=ORIENTED_EDGE('',*,*,#3969,.F.);
#5367=ORIENTED_EDGE('',*,*,#3971,.T.);
#5368=ORIENTED_EDGE('',*,*,#3972,.T.);
#5369=ORIENTED_EDGE('',*,*,#3973,.F.);
#5370=ORIENTED_EDGE('',*,*,#3972,.F.);
#5371=ORIENTED_EDGE('',*,*,#3973,.T.);
#5372=ORIENTED_EDGE('',*,*,#3974,.T.);
#5373=ORIENTED_EDGE('',*,*,#3975,.F.);
#5374=ORIENTED_EDGE('',*,*,#3974,.F.);
#5375=ORIENTED_EDGE('',*,*,#3970,.F.);
#5376=ORIENTED_EDGE('',*,*,#3975,.T.);
#5377=ORIENTED_EDGE('',*,*,#3976,.F.);
#5378=ORIENTED_EDGE('',*,*,#3977,.T.);
#5379=ORIENTED_EDGE('',*,*,#3964,.T.);
#5380=ORIENTED_EDGE('',*,*,#3965,.T.);
#5381=ORIENTED_EDGE('',*,*,#3977,.F.);
#5382=ORIENTED_EDGE('',*,*,#3976,.T.);
#5383=ORIENTED_EDGE('',*,*,#3978,.F.);
#5384=ORIENTED_EDGE('',*,*,#3978,.T.);
#5385=ORIENTED_EDGE('',*,*,#3979,.T.);
#5386=ORIENTED_EDGE('',*,*,#3971,.F.);
#5387=ORIENTED_EDGE('',*,*,#3979,.F.);
#5388=ORIENTED_EDGE('',*,*,#3980,.F.);
#5389=ORIENTED_EDGE('',*,*,#3981,.F.);
#5390=ORIENTED_EDGE('',*,*,#3982,.T.);
#5391=ORIENTED_EDGE('',*,*,#3983,.F.);
#5392=ORIENTED_EDGE('',*,*,#3984,.F.);
#5393=ORIENTED_EDGE('',*,*,#3982,.F.);
#5394=ORIENTED_EDGE('',*,*,#3985,.T.);
#5395=ORIENTED_EDGE('',*,*,#3986,.T.);
#5396=ORIENTED_EDGE('',*,*,#3983,.T.);
#5397=ORIENTED_EDGE('',*,*,#3984,.T.);
#5398=ORIENTED_EDGE('',*,*,#3986,.F.);
#5399=ORIENTED_EDGE('',*,*,#3987,.F.);
#5400=ORIENTED_EDGE('',*,*,#3988,.T.);
#5401=ORIENTED_EDGE('',*,*,#3989,.F.);
#5402=ORIENTED_EDGE('',*,*,#3990,.T.);
#5403=ORIENTED_EDGE('',*,*,#3987,.T.);
#5404=ORIENTED_EDGE('',*,*,#3990,.F.);
#5405=ORIENTED_EDGE('',*,*,#3991,.F.);
#5406=ORIENTED_EDGE('',*,*,#3992,.T.);
#5407=ORIENTED_EDGE('',*,*,#3989,.T.);
#5408=ORIENTED_EDGE('',*,*,#3992,.F.);
#5409=ORIENTED_EDGE('',*,*,#3993,.F.);
#5410=ORIENTED_EDGE('',*,*,#3994,.T.);
#5411=ORIENTED_EDGE('',*,*,#3991,.T.);
#5412=ORIENTED_EDGE('',*,*,#3994,.F.);
#5413=ORIENTED_EDGE('',*,*,#3993,.T.);
#5414=ORIENTED_EDGE('',*,*,#3985,.F.);
#5415=ORIENTED_EDGE('',*,*,#3980,.T.);
#5416=ORIENTED_EDGE('',*,*,#3981,.T.);
#5417=ORIENTED_EDGE('',*,*,#3995,.T.);
#5418=ORIENTED_EDGE('',*,*,#3988,.F.);
#5419=ORIENTED_EDGE('',*,*,#3995,.F.);
#5420=ORIENTED_EDGE('',*,*,#3996,.T.);
#5421=ORIENTED_EDGE('',*,*,#3996,.F.);
#5422=ORIENTED_EDGE('',*,*,#3997,.T.);
#5423=ORIENTED_EDGE('',*,*,#3997,.F.);
#5424=ORIENTED_EDGE('',*,*,#3998,.T.);
#5425=ORIENTED_EDGE('',*,*,#3998,.F.);
#5426=ORIENTED_EDGE('',*,*,#3999,.T.);
#5427=ORIENTED_EDGE('',*,*,#3999,.F.);
#5428=ORIENTED_EDGE('',*,*,#4000,.T.);
#5429=ORIENTED_EDGE('',*,*,#4000,.F.);
#5430=ORIENTED_EDGE('',*,*,#4001,.T.);
#5431=ORIENTED_EDGE('',*,*,#4001,.F.);
#5432=ORIENTED_EDGE('',*,*,#4002,.T.);
#5433=ORIENTED_EDGE('',*,*,#4002,.F.);
#5434=ORIENTED_EDGE('',*,*,#4003,.T.);
#5435=ORIENTED_EDGE('',*,*,#4003,.F.);
#5436=ORIENTED_EDGE('',*,*,#4004,.F.);
#5437=ORIENTED_EDGE('',*,*,#4005,.F.);
#5438=ORIENTED_EDGE('',*,*,#4006,.F.);
#5439=ORIENTED_EDGE('',*,*,#4007,.F.);
#5440=ORIENTED_EDGE('',*,*,#4006,.T.);
#5441=ORIENTED_EDGE('',*,*,#4008,.F.);
#5442=ORIENTED_EDGE('',*,*,#4009,.T.);
#5443=ORIENTED_EDGE('',*,*,#4010,.F.);
#5444=ORIENTED_EDGE('',*,*,#4011,.T.);
#5445=ORIENTED_EDGE('',*,*,#4012,.F.);
#5446=ORIENTED_EDGE('',*,*,#4013,.T.);
#5447=ORIENTED_EDGE('',*,*,#4014,.T.);
#5448=ORIENTED_EDGE('',*,*,#4015,.F.);
#5449=ORIENTED_EDGE('',*,*,#4014,.F.);
#5450=ORIENTED_EDGE('',*,*,#4016,.T.);
#5451=ORIENTED_EDGE('',*,*,#4017,.F.);
#5452=ORIENTED_EDGE('',*,*,#4018,.T.);
#5453=ORIENTED_EDGE('',*,*,#4019,.F.);
#5454=ORIENTED_EDGE('',*,*,#4020,.T.);
#5455=ORIENTED_EDGE('',*,*,#4021,.F.);
#5456=ORIENTED_EDGE('',*,*,#4022,.T.);
#5457=ORIENTED_EDGE('',*,*,#4023,.F.);
#5458=ORIENTED_EDGE('',*,*,#4024,.T.);
#5459=ORIENTED_EDGE('',*,*,#4025,.F.);
#5460=ORIENTED_EDGE('',*,*,#4005,.T.);
#5461=ORIENTED_EDGE('',*,*,#4026,.T.);
#5462=ORIENTED_EDGE('',*,*,#4027,.T.);
#5463=ORIENTED_EDGE('',*,*,#4008,.T.);
#5464=ORIENTED_EDGE('',*,*,#4028,.F.);
#5465=ORIENTED_EDGE('',*,*,#4029,.F.);
#5466=ORIENTED_EDGE('',*,*,#4009,.F.);
#5467=ORIENTED_EDGE('',*,*,#4027,.F.);
#5468=ORIENTED_EDGE('',*,*,#4029,.T.);
#5469=ORIENTED_EDGE('',*,*,#4030,.T.);
#5470=ORIENTED_EDGE('',*,*,#4031,.T.);
#5471=ORIENTED_EDGE('',*,*,#4010,.T.);
#5472=ORIENTED_EDGE('',*,*,#4032,.F.);
#5473=ORIENTED_EDGE('',*,*,#4033,.F.);
#5474=ORIENTED_EDGE('',*,*,#4011,.F.);
#5475=ORIENTED_EDGE('',*,*,#4031,.F.);
#5476=ORIENTED_EDGE('',*,*,#4033,.T.);
#5477=ORIENTED_EDGE('',*,*,#4034,.T.);
#5478=ORIENTED_EDGE('',*,*,#4035,.T.);
#5479=ORIENTED_EDGE('',*,*,#4012,.T.);
#5480=ORIENTED_EDGE('',*,*,#4036,.F.);
#5481=ORIENTED_EDGE('',*,*,#4037,.F.);
#5482=ORIENTED_EDGE('',*,*,#4016,.F.);
#5483=ORIENTED_EDGE('',*,*,#4013,.F.);
#5484=ORIENTED_EDGE('',*,*,#4035,.F.);
#5485=ORIENTED_EDGE('',*,*,#4038,.F.);
#5486=ORIENTED_EDGE('',*,*,#4037,.T.);
#5487=ORIENTED_EDGE('',*,*,#4039,.T.);
#5488=ORIENTED_EDGE('',*,*,#4040,.T.);
#5489=ORIENTED_EDGE('',*,*,#4017,.T.);
#5490=ORIENTED_EDGE('',*,*,#4041,.F.);
#5491=ORIENTED_EDGE('',*,*,#4042,.F.);
#5492=ORIENTED_EDGE('',*,*,#4018,.F.);
#5493=ORIENTED_EDGE('',*,*,#4040,.F.);
#5494=ORIENTED_EDGE('',*,*,#4042,.T.);
#5495=ORIENTED_EDGE('',*,*,#4043,.T.);
#5496=ORIENTED_EDGE('',*,*,#4044,.T.);
#5497=ORIENTED_EDGE('',*,*,#4019,.T.);
#5498=ORIENTED_EDGE('',*,*,#4045,.F.);
#5499=ORIENTED_EDGE('',*,*,#4046,.F.);
#5500=ORIENTED_EDGE('',*,*,#4020,.F.);
#5501=ORIENTED_EDGE('',*,*,#4044,.F.);
#5502=ORIENTED_EDGE('',*,*,#4046,.T.);
#5503=ORIENTED_EDGE('',*,*,#4047,.T.);
#5504=ORIENTED_EDGE('',*,*,#4048,.T.);
#5505=ORIENTED_EDGE('',*,*,#4021,.T.);
#5506=ORIENTED_EDGE('',*,*,#4022,.F.);
#5507=ORIENTED_EDGE('',*,*,#4048,.F.);
#5508=ORIENTED_EDGE('',*,*,#4049,.F.);
#5509=ORIENTED_EDGE('',*,*,#4050,.F.);
#5510=ORIENTED_EDGE('',*,*,#4051,.F.);
#5511=ORIENTED_EDGE('',*,*,#4052,.T.);
#5512=ORIENTED_EDGE('',*,*,#4038,.T.);
#5513=ORIENTED_EDGE('',*,*,#4034,.F.);
#5514=ORIENTED_EDGE('',*,*,#4032,.T.);
#5515=ORIENTED_EDGE('',*,*,#4030,.F.);
#5516=ORIENTED_EDGE('',*,*,#4028,.T.);
#5517=ORIENTED_EDGE('',*,*,#4026,.F.);
#5518=ORIENTED_EDGE('',*,*,#4004,.T.);
#5519=ORIENTED_EDGE('',*,*,#4053,.F.);
#5520=ORIENTED_EDGE('',*,*,#4054,.T.);
#5521=ORIENTED_EDGE('',*,*,#4055,.F.);
#5522=ORIENTED_EDGE('',*,*,#4049,.T.);
#5523=ORIENTED_EDGE('',*,*,#4047,.F.);
#5524=ORIENTED_EDGE('',*,*,#4045,.T.);
#5525=ORIENTED_EDGE('',*,*,#4043,.F.);
#5526=ORIENTED_EDGE('',*,*,#4041,.T.);
#5527=ORIENTED_EDGE('',*,*,#4039,.F.);
#5528=ORIENTED_EDGE('',*,*,#4036,.T.);
#5529=ORIENTED_EDGE('',*,*,#4052,.F.);
#5530=ORIENTED_EDGE('',*,*,#4007,.T.);
#5531=ORIENTED_EDGE('',*,*,#4025,.T.);
#5532=ORIENTED_EDGE('',*,*,#4056,.T.);
#5533=ORIENTED_EDGE('',*,*,#4053,.T.);
#5534=ORIENTED_EDGE('',*,*,#4024,.F.);
#5535=ORIENTED_EDGE('',*,*,#4057,.F.);
#5536=ORIENTED_EDGE('',*,*,#4054,.F.);
#5537=ORIENTED_EDGE('',*,*,#4056,.F.);
#5538=ORIENTED_EDGE('',*,*,#4015,.T.);
#5539=ORIENTED_EDGE('',*,*,#4051,.T.);
#5540=ORIENTED_EDGE('',*,*,#4050,.T.);
#5541=ORIENTED_EDGE('',*,*,#4055,.T.);
#5542=ORIENTED_EDGE('',*,*,#4057,.T.);
#5543=ORIENTED_EDGE('',*,*,#4023,.T.);
#5544=ORIENTED_EDGE('',*,*,#4058,.F.);
#5545=ORIENTED_EDGE('',*,*,#4059,.T.);
#5546=ORIENTED_EDGE('',*,*,#4060,.F.);
#5547=ORIENTED_EDGE('',*,*,#4061,.T.);
#5548=ORIENTED_EDGE('',*,*,#4058,.T.);
#5549=ORIENTED_EDGE('',*,*,#4061,.F.);
#5550=ORIENTED_EDGE('',*,*,#4060,.T.);
#5551=ORIENTED_EDGE('',*,*,#4062,.F.);
#5552=ORIENTED_EDGE('',*,*,#4062,.T.);
#5553=ORIENTED_EDGE('',*,*,#4063,.T.);
#5554=ORIENTED_EDGE('',*,*,#4059,.F.);
#5555=ORIENTED_EDGE('',*,*,#4063,.F.);
#5556=ORIENTED_EDGE('',*,*,#4064,.F.);
#5557=ORIENTED_EDGE('',*,*,#4065,.T.);
#5558=ORIENTED_EDGE('',*,*,#4066,.F.);
#5559=ORIENTED_EDGE('',*,*,#4067,.T.);
#5560=ORIENTED_EDGE('',*,*,#4064,.T.);
#5561=ORIENTED_EDGE('',*,*,#4067,.F.);
#5562=ORIENTED_EDGE('',*,*,#4066,.T.);
#5563=ORIENTED_EDGE('',*,*,#4068,.F.);
#5564=ORIENTED_EDGE('',*,*,#4068,.T.);
#5565=ORIENTED_EDGE('',*,*,#4069,.T.);
#5566=ORIENTED_EDGE('',*,*,#4065,.F.);
#5567=ORIENTED_EDGE('',*,*,#4069,.F.);
#5568=ORIENTED_EDGE('',*,*,#4070,.F.);
#5569=ORIENTED_EDGE('',*,*,#4071,.T.);
#5570=ORIENTED_EDGE('',*,*,#4072,.T.);
#5571=ORIENTED_EDGE('',*,*,#4071,.F.);
#5572=ORIENTED_EDGE('',*,*,#4073,.F.);
#5573=ORIENTED_EDGE('',*,*,#4074,.T.);
#5574=ORIENTED_EDGE('',*,*,#4075,.T.);
#5575=ORIENTED_EDGE('',*,*,#4074,.F.);
#5576=ORIENTED_EDGE('',*,*,#4073,.T.);
#5577=ORIENTED_EDGE('',*,*,#4070,.T.);
#5578=ORIENTED_EDGE('',*,*,#4075,.F.);
#5579=ORIENTED_EDGE('',*,*,#4072,.F.);
#5580=ORIENTED_EDGE('',*,*,#4076,.F.);
#5581=ORIENTED_EDGE('',*,*,#4077,.T.);
#5582=ORIENTED_EDGE('',*,*,#4078,.T.);
#5583=ORIENTED_EDGE('',*,*,#4077,.F.);
#5584=ORIENTED_EDGE('',*,*,#4079,.F.);
#5585=ORIENTED_EDGE('',*,*,#4080,.T.);
#5586=ORIENTED_EDGE('',*,*,#4081,.T.);
#5587=ORIENTED_EDGE('',*,*,#4080,.F.);
#5588=ORIENTED_EDGE('',*,*,#4079,.T.);
#5589=ORIENTED_EDGE('',*,*,#4076,.T.);
#5590=ORIENTED_EDGE('',*,*,#4081,.F.);
#5591=ORIENTED_EDGE('',*,*,#4078,.F.);
#5592=ORIENTED_EDGE('',*,*,#4082,.F.);
#5593=ORIENTED_EDGE('',*,*,#4083,.T.);
#5594=ORIENTED_EDGE('',*,*,#4084,.T.);
#5595=ORIENTED_EDGE('',*,*,#4083,.F.);
#5596=ORIENTED_EDGE('',*,*,#4085,.F.);
#5597=ORIENTED_EDGE('',*,*,#4086,.T.);
#5598=ORIENTED_EDGE('',*,*,#4087,.T.);
#5599=ORIENTED_EDGE('',*,*,#4086,.F.);
#5600=ORIENTED_EDGE('',*,*,#4085,.T.);
#5601=ORIENTED_EDGE('',*,*,#4082,.T.);
#5602=ORIENTED_EDGE('',*,*,#4087,.F.);
#5603=ORIENTED_EDGE('',*,*,#4084,.F.);
#5604=PLANE('',#6737);
#5605=PLANE('',#6738);
#5606=PLANE('',#6739);
#5607=PLANE('',#6740);
#5608=PLANE('',#6741);
#5609=PLANE('',#6742);
#5610=PLANE('',#6743);
#5611=PLANE('',#6744);
#5612=PLANE('',#6745);
#5613=PLANE('',#6746);
#5614=PLANE('',#6747);
#5615=PLANE('',#6748);
#5616=PLANE('',#6749);
#5617=PLANE('',#6750);
#5618=PLANE('',#6751);
#5619=PLANE('',#6752);
#5620=PLANE('',#6753);
#5621=PLANE('',#6754);
#5622=PLANE('',#6755);
#5623=PLANE('',#6756);
#5624=PLANE('',#6757);
#5625=PLANE('',#6758);
#5626=PLANE('',#6759);
#5627=PLANE('',#6760);
#5628=PLANE('',#6761);
#5629=PLANE('',#6762);
#5630=PLANE('',#6763);
#5631=PLANE('',#6764);
#5632=PLANE('',#6765);
#5633=PLANE('',#6766);
#5634=PLANE('',#6767);
#5635=PLANE('',#6768);
#5636=PLANE('',#6769);
#5637=PLANE('',#6770);
#5638=PLANE('',#6771);
#5639=PLANE('',#6772);
#5640=PLANE('',#6776);
#5641=PLANE('',#6777);
#5642=PLANE('',#6778);
#5643=PLANE('',#6779);
#5644=PLANE('',#6780);
#5645=PLANE('',#6781);
#5646=PLANE('',#6782);
#5647=PLANE('',#6783);
#5648=PLANE('',#6784);
#5649=PLANE('',#6785);
#5650=PLANE('',#6823);
#5651=PLANE('',#6824);
#5652=PLANE('',#6825);
#5653=PLANE('',#6826);
#5654=PLANE('',#6827);
#5655=PLANE('',#6828);
#5656=PLANE('',#6830);
#5657=PLANE('',#6831);
#5658=PLANE('',#6832);
#5659=PLANE('',#6834);
#5660=PLANE('',#6835);
#5661=PLANE('',#6836);
#5662=PLANE('',#6837);
#5663=PLANE('',#6838);
#5664=PLANE('',#6839);
#5665=PLANE('',#6846);
#5666=PLANE('',#6847);
#5667=PLANE('',#6848);
#5668=PLANE('',#6849);
#5669=PLANE('',#6856);
#5670=PLANE('',#6860);
#5671=PLANE('',#6862);
#5672=PLANE('',#6863);
#5673=PLANE('',#6864);
#5674=PLANE('',#6865);
#5675=PLANE('',#6866);
#5676=PLANE('',#6867);
#5677=PLANE('',#6869);
#5678=PLANE('',#6870);
#5679=PLANE('',#6871);
#5680=PLANE('',#6872);
#5681=PLANE('',#6873);
#5682=PLANE('',#6874);
#5683=PLANE('',#6885);
#5684=PLANE('',#6888);
#5685=PLANE('',#6893);
#5686=PLANE('',#6894);
#5687=PLANE('',#6895);
#5688=PLANE('',#6896);
#5689=PLANE('',#6897);
#5690=PLANE('',#6898);
#5691=PLANE('',#6899);
#5692=PLANE('',#6904);
#5693=PLANE('',#6905);
#5694=PLANE('',#6910);
#5695=PLANE('',#6913);
#5696=PLANE('',#6921);
#5697=PLANE('',#6922);
#5698=PLANE('',#6930);
#5699=PLANE('',#6931);
#5700=PLANE('',#6939);
#5701=PLANE('',#6940);
#5702=PLANE('',#6945);
#5703=PLANE('',#6946);
#5704=PLANE('',#6951);
#5705=PLANE('',#6954);
#5706=PLANE('',#6962);
#5707=PLANE('',#6963);
#5708=PLANE('',#6971);
#5709=PLANE('',#6972);
#5710=PLANE('',#6983);
#5711=PLANE('',#6986);
#5712=PLANE('',#6991);
#5713=PLANE('',#6992);
#5714=PLANE('',#6993);
#5715=PLANE('',#6994);
#5716=PLANE('',#6995);
#5717=PLANE('',#6996);
#5718=PLANE('',#6997);
#5719=PLANE('',#6999);
#5720=PLANE('',#7000);
#5721=PLANE('',#7001);
#5722=PLANE('',#7002);
#5723=PLANE('',#7003);
#5724=PLANE('',#7004);
#5725=PLANE('',#7005);
#5726=PLANE('',#7006);
#5727=PLANE('',#7007);
#5728=PLANE('',#7009);
#5729=PLANE('',#7017);
#5730=PLANE('',#7026);
#5731=PLANE('',#7027);
#5732=PLANE('',#7032);
#5733=PLANE('',#7035);
#5734=PLANE('',#7043);
#5735=PLANE('',#7044);
#5736=PLANE('',#7052);
#5737=PLANE('',#7053);
#5738=PLANE('',#7058);
#5739=PLANE('',#7059);
#5740=PLANE('',#7064);
#5741=PLANE('',#7067);
#5742=PLANE('',#7075);
#5743=PLANE('',#7076);
#5744=PLANE('',#7084);
#5745=PLANE('',#7085);
#5746=PLANE('',#7087);
#5747=PLANE('',#7088);
#5748=PLANE('',#7089);
#5749=PLANE('',#7090);
#5750=PLANE('',#7091);
#5751=PLANE('',#7092);
#5752=PLANE('',#7093);
#5753=PLANE('',#7094);
#5754=PLANE('',#7095);
#5755=PLANE('',#7097);
#5756=PLANE('',#7105);
#5757=PLANE('',#7114);
#5758=PLANE('',#7121);
#5759=PLANE('',#7122);
#5760=PLANE('',#7123);
#5761=PLANE('',#7124);
#5762=PLANE('',#7125);
#5763=PLANE('',#7126);
#5764=PLANE('',#7128);
#5765=PLANE('',#7129);
#5766=PLANE('',#7130);
#5767=PLANE('',#7131);
#5768=PLANE('',#7132);
#5769=PLANE('',#7133);
#5770=PLANE('',#7134);
#5771=PLANE('',#7135);
#5772=PLANE('',#7136);
#5773=PLANE('',#7138);
#5774=PLANE('',#7146);
#5775=PLANE('',#7152);
#5776=PLANE('',#7158);
#5777=PLANE('',#7159);
#5778=PLANE('',#7165);
#5779=PLANE('',#7172);
#5780=PLANE('',#7173);
#5781=PLANE('',#7174);
#5782=PLANE('',#7175);
#5783=PLANE('',#7176);
#5784=PLANE('',#7177);
#5785=PLANE('',#7179);
#5786=PLANE('',#7180);
#5787=PLANE('',#7181);
#5788=PLANE('',#7182);
#5789=PLANE('',#7183);
#5790=PLANE('',#7184);
#5791=PLANE('',#7185);
#5792=PLANE('',#7186);
#5793=PLANE('',#7194);
#5794=PLANE('',#7199);
#5795=PLANE('',#7202);
#5796=PLANE('',#7206);
#5797=PLANE('',#7207);
#5798=PLANE('',#7212);
#5799=PLANE('',#7213);
#5800=PLANE('',#7215);
#5801=PLANE('',#7216);
#5802=PLANE('',#7217);
#5803=PLANE('',#7218);
#5804=PLANE('',#7219);
#5805=PLANE('',#7224);
#5806=PLANE('',#7225);
#5807=PLANE('',#7233);
#5808=PLANE('',#7234);
#5809=PLANE('',#7242);
#5810=PLANE('',#7243);
#5811=PLANE('',#7251);
#5812=PLANE('',#7252);
#5813=PLANE('',#7317);
#5814=PLANE('',#7318);
#5815=PLANE('',#7336);
#5816=PLANE('',#7339);
#5817=PLANE('',#7351);
#5818=PLANE('',#7360);
#5819=PLANE('',#7393);
#5820=PLANE('',#7398);
#5821=PLANE('',#7403);
#5822=PLANE('',#7408);
#5823=PLANE('',#7413);
#5824=PLANE('',#7418);
#5825=PLANE('',#7427);
#5826=PLANE('',#7431);
#5827=PLANE('',#7432);
#5828=PLANE('',#7434);
#5829=PLANE('',#7439);
#5830=PLANE('',#7442);
#5831=PLANE('',#7447);
#5832=PLANE('',#7462);
#5833=PLANE('',#7463);
#5834=PLANE('',#7471);
#5835=PLANE('',#7472);
#5836=PLANE('',#7480);
#5837=PLANE('',#7481);
#5838=ADVANCED_FACE('',(#1038),#5604,.F.);
#5839=ADVANCED_FACE('',(#1039),#5605,.F.);
#5840=ADVANCED_FACE('',(#1040),#5606,.F.);
#5841=ADVANCED_FACE('',(#1041),#5607,.F.);
#5842=ADVANCED_FACE('',(#1042),#5608,.F.);
#5843=ADVANCED_FACE('',(#1043),#5609,.F.);
#5844=ADVANCED_FACE('',(#1044),#5610,.F.);
#5845=ADVANCED_FACE('',(#1045),#5611,.F.);
#5846=ADVANCED_FACE('',(#1046),#5612,.F.);
#5847=ADVANCED_FACE('',(#1047),#5613,.F.);
#5848=ADVANCED_FACE('',(#1048),#5614,.F.);
#5849=ADVANCED_FACE('',(#1049),#5615,.F.);
#5850=ADVANCED_FACE('',(#1050),#5616,.F.);
#5851=ADVANCED_FACE('',(#1051),#5617,.F.);
#5852=ADVANCED_FACE('',(#1052),#5618,.F.);
#5853=ADVANCED_FACE('',(#1053),#5619,.F.);
#5854=ADVANCED_FACE('',(#1054),#5620,.F.);
#5855=ADVANCED_FACE('',(#1055),#5621,.F.);
#5856=ADVANCED_FACE('',(#1056),#5622,.F.);
#5857=ADVANCED_FACE('',(#1057),#5623,.F.);
#5858=ADVANCED_FACE('',(#1058),#5624,.F.);
#5859=ADVANCED_FACE('',(#1059),#5625,.F.);
#5860=ADVANCED_FACE('',(#1060),#5626,.F.);
#5861=ADVANCED_FACE('',(#1061),#5627,.F.);
#5862=ADVANCED_FACE('',(#1062),#5628,.F.);
#5863=ADVANCED_FACE('',(#1063),#5629,.F.);
#5864=ADVANCED_FACE('',(#1064),#5630,.F.);
#5865=ADVANCED_FACE('',(#1065),#5631,.F.);
#5866=ADVANCED_FACE('',(#1066),#5632,.F.);
#5867=ADVANCED_FACE('',(#1067),#5633,.F.);
#5868=ADVANCED_FACE('',(#1068),#5634,.F.);
#5869=ADVANCED_FACE('',(#1069),#5635,.F.);
#5870=ADVANCED_FACE('',(#1070),#5636,.F.);
#5871=ADVANCED_FACE('',(#1071),#5637,.F.);
#5872=ADVANCED_FACE('',(#1072),#5638,.F.);
#5873=ADVANCED_FACE('',(#1073),#5639,.F.);
#5874=ADVANCED_FACE('',(#1074),#938,.F.);
#5875=ADVANCED_FACE('',(#1075),#5640,.T.);
#5876=ADVANCED_FACE('',(#1076),#5641,.T.);
#5877=ADVANCED_FACE('',(#1077),#5642,.T.);
#5878=ADVANCED_FACE('',(#1078),#5643,.T.);
#5879=ADVANCED_FACE('',(#1079),#5644,.T.);
#5880=ADVANCED_FACE('',(#1080),#5645,.T.);
#5881=ADVANCED_FACE('',(#1081),#5646,.T.);
#5882=ADVANCED_FACE('',(#1082),#5647,.T.);
#5883=ADVANCED_FACE('',(#1083,#562),#5648,.T.);
#5884=ADVANCED_FACE('',(#1084,#563),#5649,.F.);
#5885=ADVANCED_FACE('',(#1085),#939,.F.);
#5886=ADVANCED_FACE('',(#1086),#940,.F.);
#5887=ADVANCED_FACE('',(#1087),#941,.F.);
#5888=ADVANCED_FACE('',(#1088),#942,.F.);
#5889=ADVANCED_FACE('',(#1089),#943,.F.);
#5890=ADVANCED_FACE('',(#1090),#944,.F.);
#5891=ADVANCED_FACE('',(#1091),#945,.F.);
#5892=ADVANCED_FACE('',(#1092),#946,.F.);
#5893=ADVANCED_FACE('',(#1093),#947,.F.);
#5894=ADVANCED_FACE('',(#1094),#948,.F.);
#5895=ADVANCED_FACE('',(#1095),#949,.F.);
#5896=ADVANCED_FACE('',(#1096),#950,.F.);
#5897=ADVANCED_FACE('',(#1097),#5650,.T.);
#5898=ADVANCED_FACE('',(#1098),#5651,.T.);
#5899=ADVANCED_FACE('',(#1099),#5652,.T.);
#5900=ADVANCED_FACE('',(#1100),#5653,.T.);
#5901=ADVANCED_FACE('',(#1101,#564,#565,#566,#567,#568,#569,#570,#571,#572,
#573,#574,#575),#5654,.T.);
#5902=ADVANCED_FACE('',(#1102,#576,#577,#578,#579,#580,#581,#582,#583,#584,
#585,#586,#587),#5655,.F.);
#5903=ADVANCED_FACE('',(#1103),#5656,.F.);
#5904=ADVANCED_FACE('',(#1104),#5657,.T.);
#5905=ADVANCED_FACE('',(#1105,#588),#5658,.T.);
#5906=ADVANCED_FACE('',(#1106),#5659,.T.);
#5907=ADVANCED_FACE('',(#1107),#5660,.T.);
#5908=ADVANCED_FACE('',(#1108),#5661,.F.);
#5909=ADVANCED_FACE('',(#1109),#5662,.T.);
#5910=ADVANCED_FACE('',(#1110),#5663,.T.);
#5911=ADVANCED_FACE('',(#1111),#5664,.T.);
#5912=ADVANCED_FACE('',(#1112),#951,.F.);
#5913=ADVANCED_FACE('',(#1113),#5665,.F.);
#5914=ADVANCED_FACE('',(#1114),#5666,.F.);
#5915=ADVANCED_FACE('',(#1115),#5667,.T.);
#5916=ADVANCED_FACE('',(#1116),#5668,.T.);
#5917=ADVANCED_FACE('',(#1117),#359,.F.);
#5918=ADVANCED_FACE('',(#1118),#952,.F.);
#5919=ADVANCED_FACE('',(#1119,#589),#5669,.T.);
#5920=ADVANCED_FACE('',(#1120),#953,.T.);
#5921=ADVANCED_FACE('',(#1121,#590),#5670,.F.);
#5922=ADVANCED_FACE('',(#1122),#5671,.T.);
#5923=ADVANCED_FACE('',(#1123),#5672,.T.);
#5924=ADVANCED_FACE('',(#1124),#5673,.T.);
#5925=ADVANCED_FACE('',(#1125),#5674,.T.);
#5926=ADVANCED_FACE('',(#1126),#5675,.T.);
#5927=ADVANCED_FACE('',(#1127),#5676,.F.);
#5928=ADVANCED_FACE('',(#1128),#5677,.T.);
#5929=ADVANCED_FACE('',(#1129),#5678,.T.);
#5930=ADVANCED_FACE('',(#1130),#5679,.T.);
#5931=ADVANCED_FACE('',(#1131),#5680,.T.);
#5932=ADVANCED_FACE('',(#1132),#5681,.T.);
#5933=ADVANCED_FACE('',(#1133),#5682,.F.);
#5934=ADVANCED_FACE('',(#1134),#954,.F.);
#5935=ADVANCED_FACE('',(#1135),#955,.F.);
#5936=ADVANCED_FACE('',(#1136),#956,.F.);
#5937=ADVANCED_FACE('',(#1137,#591,#592),#5683,.T.);
#5938=ADVANCED_FACE('',(#1138),#5684,.T.);
#5939=ADVANCED_FACE('',(#1139),#957,.F.);
#5940=ADVANCED_FACE('',(#1140),#958,.F.);
#5941=ADVANCED_FACE('',(#1141,#593,#594),#5685,.T.);
#5942=ADVANCED_FACE('',(#1142),#5686,.F.);
#5943=ADVANCED_FACE('',(#1143),#5687,.T.);
#5944=ADVANCED_FACE('',(#1144,#595,#596),#5688,.T.);
#5945=ADVANCED_FACE('',(#1145),#5689,.T.);
#5946=ADVANCED_FACE('',(#1146),#5690,.T.);
#5947=ADVANCED_FACE('',(#1147,#597,#598),#5691,.F.);
#5948=ADVANCED_FACE('',(#1148),#959,.F.);
#5949=ADVANCED_FACE('',(#1149),#5692,.T.);
#5950=ADVANCED_FACE('',(#1150,#599),#5693,.T.);
#5951=ADVANCED_FACE('',(#1151),#960,.T.);
#5952=ADVANCED_FACE('',(#1152),#5694,.F.);
#5953=ADVANCED_FACE('',(#1153),#961,.T.);
#5954=ADVANCED_FACE('',(#1154,#600),#5695,.T.);
#5955=ADVANCED_FACE('',(#1155),#962,.F.);
#5956=ADVANCED_FACE('',(#1156),#963,.T.);
#5957=ADVANCED_FACE('',(#1157,#601),#5696,.T.);
#5958=ADVANCED_FACE('',(#1158,#602),#5697,.F.);
#5959=ADVANCED_FACE('',(#1159),#964,.F.);
#5960=ADVANCED_FACE('',(#1160),#965,.T.);
#5961=ADVANCED_FACE('',(#1161,#603),#5698,.T.);
#5962=ADVANCED_FACE('',(#1162,#604),#5699,.F.);
#5963=ADVANCED_FACE('',(#1163),#966,.F.);
#5964=ADVANCED_FACE('',(#1164),#967,.T.);
#5965=ADVANCED_FACE('',(#1165,#605),#5700,.T.);
#5966=ADVANCED_FACE('',(#1166,#606),#5701,.F.);
#5967=ADVANCED_FACE('',(#1167),#968,.F.);
#5968=ADVANCED_FACE('',(#1168),#5702,.T.);
#5969=ADVANCED_FACE('',(#1169,#607),#5703,.T.);
#5970=ADVANCED_FACE('',(#1170),#969,.T.);
#5971=ADVANCED_FACE('',(#1171),#5704,.F.);
#5972=ADVANCED_FACE('',(#1172),#970,.T.);
#5973=ADVANCED_FACE('',(#1173,#608),#5705,.T.);
#5974=ADVANCED_FACE('',(#1174),#971,.F.);
#5975=ADVANCED_FACE('',(#1175),#972,.T.);
#5976=ADVANCED_FACE('',(#1176,#609),#5706,.T.);
#5977=ADVANCED_FACE('',(#1177,#610),#5707,.F.);
#5978=ADVANCED_FACE('',(#1178),#973,.F.);
#5979=ADVANCED_FACE('',(#1179),#974,.T.);
#5980=ADVANCED_FACE('',(#1180,#611),#5708,.T.);
#5981=ADVANCED_FACE('',(#1181,#612),#5709,.F.);
#5982=ADVANCED_FACE('',(#1182),#975,.F.);
#5983=ADVANCED_FACE('',(#1183),#976,.F.);
#5984=ADVANCED_FACE('',(#1184),#977,.F.);
#5985=ADVANCED_FACE('',(#1185,#613,#614),#5710,.T.);
#5986=ADVANCED_FACE('',(#1186),#5711,.T.);
#5987=ADVANCED_FACE('',(#1187),#978,.F.);
#5988=ADVANCED_FACE('',(#1188),#979,.F.);
#5989=ADVANCED_FACE('',(#1189,#615,#616),#5712,.T.);
#5990=ADVANCED_FACE('',(#1190),#5713,.F.);
#5991=ADVANCED_FACE('',(#1191),#5714,.T.);
#5992=ADVANCED_FACE('',(#1192,#617,#618),#5715,.T.);
#5993=ADVANCED_FACE('',(#1193),#5716,.T.);
#5994=ADVANCED_FACE('',(#1194),#5717,.T.);
#5995=ADVANCED_FACE('',(#1195,#619,#620),#5718,.F.);
#5996=ADVANCED_FACE('',(#1196),#5719,.F.);
#5997=ADVANCED_FACE('',(#1197),#5720,.F.);
#5998=ADVANCED_FACE('',(#1198),#5721,.F.);
#5999=ADVANCED_FACE('',(#1199),#5722,.F.);
#6000=ADVANCED_FACE('',(#1200),#5723,.F.);
#6001=ADVANCED_FACE('',(#1201),#5724,.F.);
#6002=ADVANCED_FACE('',(#1202),#5725,.F.);
#6003=ADVANCED_FACE('',(#1203),#5726,.F.);
#6004=ADVANCED_FACE('',(#1204),#5727,.F.);
#6005=ADVANCED_FACE('',(#1205),#5728,.T.);
#6006=ADVANCED_FACE('',(#1206),#360,.T.);
#6007=ADVANCED_FACE('',(#1207),#980,.T.);
#6008=ADVANCED_FACE('',(#1208),#361,.T.);
#6009=ADVANCED_FACE('',(#1209,#621),#5729,.T.);
#6010=ADVANCED_FACE('',(#1210),#362,.T.);
#6011=ADVANCED_FACE('',(#1211),#981,.T.);
#6012=ADVANCED_FACE('',(#1212),#982,.F.);
#6013=ADVANCED_FACE('',(#1213),#5730,.T.);
#6014=ADVANCED_FACE('',(#1214,#622),#5731,.T.);
#6015=ADVANCED_FACE('',(#1215),#983,.T.);
#6016=ADVANCED_FACE('',(#1216),#5732,.F.);
#6017=ADVANCED_FACE('',(#1217),#984,.T.);
#6018=ADVANCED_FACE('',(#1218,#623),#5733,.T.);
#6019=ADVANCED_FACE('',(#1219),#985,.F.);
#6020=ADVANCED_FACE('',(#1220),#986,.T.);
#6021=ADVANCED_FACE('',(#1221,#624),#5734,.T.);
#6022=ADVANCED_FACE('',(#1222,#625),#5735,.F.);
#6023=ADVANCED_FACE('',(#1223),#987,.F.);
#6024=ADVANCED_FACE('',(#1224),#988,.T.);
#6025=ADVANCED_FACE('',(#1225,#626),#5736,.T.);
#6026=ADVANCED_FACE('',(#1226,#627),#5737,.F.);
#6027=ADVANCED_FACE('',(#1227),#989,.F.);
#6028=ADVANCED_FACE('',(#1228),#5738,.T.);
#6029=ADVANCED_FACE('',(#1229,#628),#5739,.T.);
#6030=ADVANCED_FACE('',(#1230),#990,.T.);
#6031=ADVANCED_FACE('',(#1231),#5740,.F.);
#6032=ADVANCED_FACE('',(#1232),#991,.T.);
#6033=ADVANCED_FACE('',(#1233,#629),#5741,.T.);
#6034=ADVANCED_FACE('',(#1234),#992,.F.);
#6035=ADVANCED_FACE('',(#1235),#993,.T.);
#6036=ADVANCED_FACE('',(#1236,#630),#5742,.T.);
#6037=ADVANCED_FACE('',(#1237,#631),#5743,.F.);
#6038=ADVANCED_FACE('',(#1238),#994,.F.);
#6039=ADVANCED_FACE('',(#1239),#995,.T.);
#6040=ADVANCED_FACE('',(#1240,#632),#5744,.T.);
#6041=ADVANCED_FACE('',(#1241,#633),#5745,.F.);
#6042=ADVANCED_FACE('',(#1242),#5746,.F.);
#6043=ADVANCED_FACE('',(#1243),#5747,.F.);
#6044=ADVANCED_FACE('',(#1244),#5748,.F.);
#6045=ADVANCED_FACE('',(#1245),#5749,.F.);
#6046=ADVANCED_FACE('',(#1246),#5750,.F.);
#6047=ADVANCED_FACE('',(#1247),#5751,.F.);
#6048=ADVANCED_FACE('',(#1248),#5752,.F.);
#6049=ADVANCED_FACE('',(#1249),#5753,.F.);
#6050=ADVANCED_FACE('',(#1250),#5754,.F.);
#6051=ADVANCED_FACE('',(#1251),#5755,.T.);
#6052=ADVANCED_FACE('',(#1252),#363,.T.);
#6053=ADVANCED_FACE('',(#1253),#996,.T.);
#6054=ADVANCED_FACE('',(#1254),#364,.T.);
#6055=ADVANCED_FACE('',(#1255,#634),#5756,.T.);
#6056=ADVANCED_FACE('',(#1256),#365,.T.);
#6057=ADVANCED_FACE('',(#1257),#997,.T.);
#6058=ADVANCED_FACE('',(#1258),#998,.T.);
#6059=ADVANCED_FACE('',(#1259),#5757,.T.);
#6060=ADVANCED_FACE('',(#1260),#999,.F.);
#6061=ADVANCED_FACE('',(#1261),#1000,.F.);
#6062=ADVANCED_FACE('',(#1262),#5758,.T.);
#6063=ADVANCED_FACE('',(#1263),#5759,.T.);
#6064=ADVANCED_FACE('',(#1264),#5760,.T.);
#6065=ADVANCED_FACE('',(#1265),#5761,.T.);
#6066=ADVANCED_FACE('',(#1266,#635,#636,#637),#5762,.T.);
#6067=ADVANCED_FACE('',(#1267,#638,#639),#5763,.F.);
#6068=ADVANCED_FACE('',(#1268),#5764,.F.);
#6069=ADVANCED_FACE('',(#1269),#5765,.F.);
#6070=ADVANCED_FACE('',(#1270),#5766,.F.);
#6071=ADVANCED_FACE('',(#1271),#5767,.F.);
#6072=ADVANCED_FACE('',(#1272),#5768,.F.);
#6073=ADVANCED_FACE('',(#1273),#5769,.F.);
#6074=ADVANCED_FACE('',(#1274),#5770,.F.);
#6075=ADVANCED_FACE('',(#1275),#5771,.F.);
#6076=ADVANCED_FACE('',(#1276),#5772,.F.);
#6077=ADVANCED_FACE('',(#1277),#5773,.T.);
#6078=ADVANCED_FACE('',(#1278),#366,.T.);
#6079=ADVANCED_FACE('',(#1279),#1001,.T.);
#6080=ADVANCED_FACE('',(#1280),#367,.T.);
#6081=ADVANCED_FACE('',(#1281,#640),#5774,.T.);
#6082=ADVANCED_FACE('',(#1282),#368,.T.);
#6083=ADVANCED_FACE('',(#1283),#1002,.T.);
#6084=ADVANCED_FACE('',(#1284),#5775,.T.);
#6085=ADVANCED_FACE('',(#1285),#1003,.F.);
#6086=ADVANCED_FACE('',(#1286),#5776,.T.);
#6087=ADVANCED_FACE('',(#1287),#5777,.T.);
#6088=ADVANCED_FACE('',(#1288),#1004,.F.);
#6089=ADVANCED_FACE('',(#1289),#5778,.T.);
#6090=ADVANCED_FACE('',(#1290,#641),#1005,.F.);
#6091=ADVANCED_FACE('',(#1291,#642),#1006,.F.);
#6092=ADVANCED_FACE('',(#1292,#643,#644),#5779,.T.);
#6093=ADVANCED_FACE('',(#1293),#5780,.T.);
#6094=ADVANCED_FACE('',(#1294),#5781,.T.);
#6095=ADVANCED_FACE('',(#1295),#5782,.T.);
#6096=ADVANCED_FACE('',(#1296,#645,#646),#5783,.T.);
#6097=ADVANCED_FACE('',(#1297,#647,#648),#5784,.F.);
#6098=ADVANCED_FACE('',(#1298),#5785,.F.);
#6099=ADVANCED_FACE('',(#1299),#5786,.F.);
#6100=ADVANCED_FACE('',(#1300),#5787,.F.);
#6101=ADVANCED_FACE('',(#1301),#5788,.F.);
#6102=ADVANCED_FACE('',(#1302),#5789,.F.);
#6103=ADVANCED_FACE('',(#1303),#5790,.F.);
#6104=ADVANCED_FACE('',(#1304),#5791,.F.);
#6105=ADVANCED_FACE('',(#1305,#649),#5792,.T.);
#6106=ADVANCED_FACE('',(#1306),#369,.T.);
#6107=ADVANCED_FACE('',(#1307),#1007,.T.);
#6108=ADVANCED_FACE('',(#1308),#370,.T.);
#6109=ADVANCED_FACE('',(#1309),#5793,.T.);
#6110=ADVANCED_FACE('',(#1310),#1008,.F.);
#6111=ADVANCED_FACE('',(#1311),#5794,.F.);
#6112=ADVANCED_FACE('',(#1312),#1009,.T.);
#6113=ADVANCED_FACE('',(#1313,#650),#5795,.F.);
#6114=ADVANCED_FACE('',(#1314,#651),#1010,.T.);
#6115=ADVANCED_FACE('',(#1315),#5796,.T.);
#6116=ADVANCED_FACE('',(#1316),#5797,.F.);
#6117=ADVANCED_FACE('',(#1317),#1011,.T.);
#6118=ADVANCED_FACE('',(#1318),#5798,.T.);
#6119=ADVANCED_FACE('',(#1319),#5799,.F.);
#6120=ADVANCED_FACE('',(#1320),#5800,.T.);
#6121=ADVANCED_FACE('',(#1321),#5801,.T.);
#6122=ADVANCED_FACE('',(#1322),#5802,.T.);
#6123=ADVANCED_FACE('',(#1323),#5803,.T.);
#6124=ADVANCED_FACE('',(#1324),#5804,.F.);
#6125=ADVANCED_FACE('',(#1325),#1012,.T.);
#6126=ADVANCED_FACE('',(#1326),#5805,.T.);
#6127=ADVANCED_FACE('',(#1327),#5806,.F.);
#6128=ADVANCED_FACE('',(#1328),#1013,.F.);
#6129=ADVANCED_FACE('',(#1329),#1014,.T.);
#6130=ADVANCED_FACE('',(#1330,#652),#5807,.T.);
#6131=ADVANCED_FACE('',(#1331,#653),#5808,.F.);
#6132=ADVANCED_FACE('',(#1332),#1015,.F.);
#6133=ADVANCED_FACE('',(#1333),#1016,.T.);
#6134=ADVANCED_FACE('',(#1334,#654),#5809,.T.);
#6135=ADVANCED_FACE('',(#1335,#655),#5810,.F.);
#6136=ADVANCED_FACE('',(#1336),#1017,.F.);
#6137=ADVANCED_FACE('',(#1337),#1018,.T.);
#6138=ADVANCED_FACE('',(#1338,#656),#5811,.T.);
#6139=ADVANCED_FACE('',(#1339,#657),#5812,.F.);
#6140=ADVANCED_FACE('',(#1340),#1019,.T.);
#6141=ADVANCED_FACE('',(#1341),#5813,.T.);
#6142=ADVANCED_FACE('',(#1342),#5814,.F.);
#6143=ADVANCED_FACE('',(#1343),#27,.F.);
#6144=ADVANCED_FACE('',(#1344),#1020,.T.);
#6145=ADVANCED_FACE('',(#1345),#1021,.F.);
#6146=ADVANCED_FACE('',(#1346),#371,.F.);
#6147=ADVANCED_FACE('',(#1347,#658),#5815,.T.);
#6148=ADVANCED_FACE('',(#1348),#1022,.T.);
#6149=ADVANCED_FACE('',(#1349,#659),#5816,.T.);
#6150=ADVANCED_FACE('',(#1350),#372,.F.);
#6151=ADVANCED_FACE('',(#1351),#28,.F.);
#6152=ADVANCED_FACE('',(#1352),#1023,.F.);
#6153=ADVANCED_FACE('',(#1353,#660),#5817,.T.);
#6154=ADVANCED_FACE('',(#1354),#373,.T.);
#6155=ADVANCED_FACE('',(#1355),#1024,.T.);
#6156=ADVANCED_FACE('',(#1356),#374,.T.);
#6157=ADVANCED_FACE('',(#1357,#661),#5818,.T.);
#6158=ADVANCED_FACE('',(#1358),#1025,.F.);
#6159=ADVANCED_FACE('',(#1359),#11,.T.);
#6160=ADVANCED_FACE('',(#1360),#12,.T.);
#6161=ADVANCED_FACE('',(#1361),#13,.T.);
#6162=ADVANCED_FACE('',(#1362),#14,.T.);
#6163=ADVANCED_FACE('',(#1363),#15,.T.);
#6164=ADVANCED_FACE('',(#1364),#16,.T.);
#6165=ADVANCED_FACE('',(#1365),#17,.T.);
#6166=ADVANCED_FACE('',(#1366),#18,.T.);
#6167=ADVANCED_FACE('',(#1367),#19,.F.);
#6168=ADVANCED_FACE('',(#1368),#1026,.T.);
#6169=ADVANCED_FACE('',(#1369),#5819,.T.);
#6170=ADVANCED_FACE('',(#1370),#20,.F.);
#6171=ADVANCED_FACE('',(#1371),#5820,.T.);
#6172=ADVANCED_FACE('',(#1372),#21,.F.);
#6173=ADVANCED_FACE('',(#1373),#5821,.T.);
#6174=ADVANCED_FACE('',(#1374),#22,.F.);
#6175=ADVANCED_FACE('',(#1375),#5822,.T.);
#6176=ADVANCED_FACE('',(#1376),#23,.F.);
#6177=ADVANCED_FACE('',(#1377),#5823,.T.);
#6178=ADVANCED_FACE('',(#1378),#24,.F.);
#6179=ADVANCED_FACE('',(#1379),#5824,.T.);
#6180=ADVANCED_FACE('',(#1380),#25,.F.);
#6181=ADVANCED_FACE('',(#1381),#1027,.F.);
#6182=ADVANCED_FACE('',(#1382),#5825,.T.);
#6183=ADVANCED_FACE('',(#1383),#26,.F.);
#6184=ADVANCED_FACE('',(#1384,#662),#5826,.T.);
#6185=ADVANCED_FACE('',(#1385),#5827,.T.);
#6186=ADVANCED_FACE('',(#1386,#663),#5828,.T.);
#6187=ADVANCED_FACE('',(#1387),#1028,.T.);
#6188=ADVANCED_FACE('',(#1388,#664),#5829,.T.);
#6189=ADVANCED_FACE('',(#1389),#1029,.F.);
#6190=ADVANCED_FACE('',(#1390,#665),#5830,.T.);
#6191=ADVANCED_FACE('',(#1391),#1030,.T.);
#6192=ADVANCED_FACE('',(#1392,#666),#5831,.T.);
#6193=ADVANCED_FACE('',(#1393),#1031,.F.);
#6194=ADVANCED_FACE('',(#1394),#1032,.F.);
#6195=ADVANCED_FACE('',(#1395),#1033,.T.);
#6196=ADVANCED_FACE('',(#1396,#667),#5832,.T.);
#6197=ADVANCED_FACE('',(#1397,#668),#5833,.F.);
#6198=ADVANCED_FACE('',(#1398),#1034,.F.);
#6199=ADVANCED_FACE('',(#1399),#1035,.T.);
#6200=ADVANCED_FACE('',(#1400,#669),#5834,.T.);
#6201=ADVANCED_FACE('',(#1401,#670),#5835,.F.);
#6202=ADVANCED_FACE('',(#1402),#1036,.F.);
#6203=ADVANCED_FACE('',(#1403),#1037,.T.);
#6204=ADVANCED_FACE('',(#1404,#671),#5836,.T.);
#6205=ADVANCED_FACE('',(#1405,#672),#5837,.F.);
#6206=CLOSED_SHELL('',(#5838,#5839,#5840,#5841,#5842,#5843,#5844,#5845,
#5846,#5847,#5848,#5849,#5850,#5851,#5852,#5853,#5854,#5855,#5856,#5857,
#5858,#5859,#5860,#5861,#5862,#5863,#5864,#5865,#5866,#5867,#5868,#5869,
#5870,#5871,#5872,#5873,#5874,#5875,#5876,#5877,#5878,#5879,#5880,#5881,
#5882,#5883,#5884));
#6207=CLOSED_SHELL('',(#5885,#5886,#5887,#5888,#5889,#5890,#5891,#5892,
#5893,#5894,#5895,#5896,#5897,#5898,#5899,#5900,#5901,#5902));
#6208=CLOSED_SHELL('',(#5903,#5904,#5905,#5906,#5907,#5908,#5909,#5910,
#5911,#5912,#5913,#5914,#5915,#5916));
#6209=CLOSED_SHELL('',(#5917,#5918,#5919,#5920,#5921));
#6210=CLOSED_SHELL('',(#5922,#5923,#5924,#5925,#5926,#5927));
#6211=CLOSED_SHELL('',(#5928,#5929,#5930,#5931,#5932,#5933));
#6212=CLOSED_SHELL('',(#5934,#5935,#5936,#5937,#5938,#5939,#5940,#5941,
#5942,#5943,#5944,#5945,#5946,#5947));
#6213=CLOSED_SHELL('',(#5948,#5949,#5950,#5951,#5952,#5953,#5954));
#6214=CLOSED_SHELL('',(#5955,#5956,#5957,#5958));
#6215=CLOSED_SHELL('',(#5959,#5960,#5961,#5962));
#6216=CLOSED_SHELL('',(#5963,#5964,#5965,#5966));
#6217=CLOSED_SHELL('',(#5967,#5968,#5969,#5970,#5971,#5972,#5973));
#6218=CLOSED_SHELL('',(#5974,#5975,#5976,#5977));
#6219=CLOSED_SHELL('',(#5978,#5979,#5980,#5981));
#6220=CLOSED_SHELL('',(#5982,#5983,#5984,#5985,#5986,#5987,#5988,#5989,
#5990,#5991,#5992,#5993,#5994,#5995));
#6221=CLOSED_SHELL('',(#5996,#5997,#5998,#5999,#6000,#6001,#6002,#6003));
#6222=CLOSED_SHELL('',(#6004,#6005,#6006,#6007,#6008,#6009,#6010,#6011));
#6223=CLOSED_SHELL('',(#6012,#6013,#6014,#6015,#6016,#6017,#6018));
#6224=CLOSED_SHELL('',(#6019,#6020,#6021,#6022));
#6225=CLOSED_SHELL('',(#6023,#6024,#6025,#6026));
#6226=CLOSED_SHELL('',(#6027,#6028,#6029,#6030,#6031,#6032,#6033));
#6227=CLOSED_SHELL('',(#6034,#6035,#6036,#6037));
#6228=CLOSED_SHELL('',(#6038,#6039,#6040,#6041));
#6229=CLOSED_SHELL('',(#6042,#6043,#6044,#6045,#6046,#6047,#6048,#6049));
#6230=CLOSED_SHELL('',(#6050,#6051,#6052,#6053,#6054,#6055,#6056,#6057));
#6231=CLOSED_SHELL('',(#6058,#6059,#6060,#6061,#6062,#6063,#6064,#6065,
#6066,#6067));
#6232=CLOSED_SHELL('',(#6068,#6069,#6070,#6071,#6072,#6073,#6074,#6075));
#6233=CLOSED_SHELL('',(#6076,#6077,#6078,#6079,#6080,#6081,#6082,#6083));
#6234=CLOSED_SHELL('',(#6084,#6085,#6086,#6087,#6088,#6089,#6090,#6091,
#6092,#6093,#6094,#6095,#6096,#6097));
#6235=CLOSED_SHELL('',(#6098,#6099,#6100,#6101,#6102,#6103,#6104,#6105,
#6106,#6107,#6108,#6109));
#6236=CLOSED_SHELL('',(#6110,#6111,#6112,#6113,#6114,#6115,#6116));
#6237=CLOSED_SHELL('',(#6117,#6118,#6119));
#6238=CLOSED_SHELL('',(#6120,#6121,#6122,#6123,#6124));
#6239=CLOSED_SHELL('',(#6125,#6126,#6127));
#6240=CLOSED_SHELL('',(#6128,#6129,#6130,#6131));
#6241=CLOSED_SHELL('',(#6132,#6133,#6134,#6135));
#6242=CLOSED_SHELL('',(#6136,#6137,#6138,#6139));
#6243=CLOSED_SHELL('',(#6140,#6141,#6142));
#6244=CLOSED_SHELL('',(#6143,#6144,#6145,#6146,#6147,#6148,#6149,#6150));
#6245=CLOSED_SHELL('',(#6151,#6152,#6153,#6154,#6155,#6156,#6157,#6158));
#6246=CLOSED_SHELL('',(#6159));
#6247=CLOSED_SHELL('',(#6160));
#6248=CLOSED_SHELL('',(#6161));
#6249=CLOSED_SHELL('',(#6162));
#6250=CLOSED_SHELL('',(#6163));
#6251=CLOSED_SHELL('',(#6164));
#6252=CLOSED_SHELL('',(#6165));
#6253=CLOSED_SHELL('',(#6166));
#6254=CLOSED_SHELL('',(#6167,#6168,#6169,#6170,#6171,#6172,#6173,#6174,
#6175,#6176,#6177,#6178,#6179,#6180,#6181,#6182,#6183,#6184,#6185));
#6255=CLOSED_SHELL('',(#6186,#6187,#6188,#6189));
#6256=CLOSED_SHELL('',(#6190,#6191,#6192,#6193));
#6257=CLOSED_SHELL('',(#6194,#6195,#6196,#6197));
#6258=CLOSED_SHELL('',(#6198,#6199,#6200,#6201));
#6259=CLOSED_SHELL('',(#6202,#6203,#6204,#6205));
#6260=DERIVED_UNIT_ELEMENT(#6346,1.);
#6261=DERIVED_UNIT_ELEMENT(#11750,-3.);
#6262=DERIVED_UNIT_ELEMENT(#6346,1.);
#6263=DERIVED_UNIT_ELEMENT(#11750,-3.);
#6264=DERIVED_UNIT_ELEMENT(#6346,1.);
#6265=DERIVED_UNIT_ELEMENT(#11750,-3.);
#6266=DERIVED_UNIT_ELEMENT(#6346,1.);
#6267=DERIVED_UNIT_ELEMENT(#11750,-3.);
#6268=DERIVED_UNIT_ELEMENT(#6346,1.);
#6269=DERIVED_UNIT_ELEMENT(#11750,-3.);
#6270=DERIVED_UNIT_ELEMENT(#6346,1.);
#6271=DERIVED_UNIT_ELEMENT(#11750,-3.);
#6272=DERIVED_UNIT_ELEMENT(#6346,1.);
#6273=DERIVED_UNIT_ELEMENT(#11750,-3.);
#6274=DERIVED_UNIT_ELEMENT(#6346,1.);
#6275=DERIVED_UNIT_ELEMENT(#11750,-3.);
#6276=DERIVED_UNIT_ELEMENT(#6346,1.);
#6277=DERIVED_UNIT_ELEMENT(#11750,-3.);
#6278=DERIVED_UNIT_ELEMENT(#6346,1.);
#6279=DERIVED_UNIT_ELEMENT(#11750,-3.);
#6280=DERIVED_UNIT_ELEMENT(#6346,1.);
#6281=DERIVED_UNIT_ELEMENT(#11750,-3.);
#6282=DERIVED_UNIT_ELEMENT(#6346,1.);
#6283=DERIVED_UNIT_ELEMENT(#11750,-3.);
#6284=DERIVED_UNIT_ELEMENT(#6346,1.);
#6285=DERIVED_UNIT_ELEMENT(#11750,-3.);
#6286=DERIVED_UNIT_ELEMENT(#6346,1.);
#6287=DERIVED_UNIT_ELEMENT(#11750,-3.);
#6288=DERIVED_UNIT_ELEMENT(#6346,1.);
#6289=DERIVED_UNIT_ELEMENT(#11750,-3.);
#6290=DERIVED_UNIT_ELEMENT(#6346,1.);
#6291=DERIVED_UNIT_ELEMENT(#11750,-3.);
#6292=DERIVED_UNIT_ELEMENT(#6346,1.);
#6293=DERIVED_UNIT_ELEMENT(#11750,-3.);
#6294=DERIVED_UNIT_ELEMENT(#6346,1.);
#6295=DERIVED_UNIT_ELEMENT(#11750,-3.);
#6296=DERIVED_UNIT_ELEMENT(#6346,1.);
#6297=DERIVED_UNIT_ELEMENT(#11750,-3.);
#6298=DERIVED_UNIT_ELEMENT(#6346,1.);
#6299=DERIVED_UNIT_ELEMENT(#11750,-3.);
#6300=DERIVED_UNIT_ELEMENT(#6346,1.);
#6301=DERIVED_UNIT_ELEMENT(#11750,-3.);
#6302=DERIVED_UNIT_ELEMENT(#6346,1.);
#6303=DERIVED_UNIT_ELEMENT(#11750,-3.);
#6304=DERIVED_UNIT_ELEMENT(#6346,1.);
#6305=DERIVED_UNIT_ELEMENT(#11750,-3.);
#6306=DERIVED_UNIT_ELEMENT(#6346,1.);
#6307=DERIVED_UNIT_ELEMENT(#11750,-3.);
#6308=DERIVED_UNIT_ELEMENT(#6346,1.);
#6309=DERIVED_UNIT_ELEMENT(#11750,-3.);
#6310=DERIVED_UNIT_ELEMENT(#6346,1.);
#6311=DERIVED_UNIT_ELEMENT(#11750,-3.);
#6312=DERIVED_UNIT_ELEMENT(#6346,1.);
#6313=DERIVED_UNIT_ELEMENT(#11750,-3.);
#6314=DERIVED_UNIT_ELEMENT(#6346,1.);
#6315=DERIVED_UNIT_ELEMENT(#11750,-3.);
#6316=DERIVED_UNIT_ELEMENT(#6346,1.);
#6317=DERIVED_UNIT_ELEMENT(#11750,-3.);
#6318=DERIVED_UNIT_ELEMENT(#6346,1.);
#6319=DERIVED_UNIT_ELEMENT(#11750,-3.);
#6320=DERIVED_UNIT_ELEMENT(#6346,1.);
#6321=DERIVED_UNIT_ELEMENT(#11750,-3.);
#6322=DERIVED_UNIT_ELEMENT(#6346,1.);
#6323=DERIVED_UNIT_ELEMENT(#11750,-3.);
#6324=DERIVED_UNIT_ELEMENT(#6346,1.);
#6325=DERIVED_UNIT_ELEMENT(#11750,-3.);
#6326=DERIVED_UNIT_ELEMENT(#6346,1.);
#6327=DERIVED_UNIT_ELEMENT(#11750,-3.);
#6328=DERIVED_UNIT_ELEMENT(#6346,1.);
#6329=DERIVED_UNIT_ELEMENT(#11750,-3.);
#6330=DERIVED_UNIT_ELEMENT(#6346,1.);
#6331=DERIVED_UNIT_ELEMENT(#11750,-3.);
#6332=DERIVED_UNIT_ELEMENT(#6346,1.);
#6333=DERIVED_UNIT_ELEMENT(#11750,-3.);
#6334=DERIVED_UNIT_ELEMENT(#6346,1.);
#6335=DERIVED_UNIT_ELEMENT(#11750,-3.);
#6336=DERIVED_UNIT_ELEMENT(#6346,1.);
#6337=DERIVED_UNIT_ELEMENT(#11750,-3.);
#6338=DERIVED_UNIT_ELEMENT(#6346,1.);
#6339=DERIVED_UNIT_ELEMENT(#11750,-3.);
#6340=DERIVED_UNIT_ELEMENT(#6346,1.);
#6341=DERIVED_UNIT_ELEMENT(#11750,-3.);
#6342=DERIVED_UNIT_ELEMENT(#6346,1.);
#6343=DERIVED_UNIT_ELEMENT(#11750,-3.);
#6344=DERIVED_UNIT_ELEMENT(#6346,1.);
#6345=DERIVED_UNIT_ELEMENT(#11750,-3.);
#6346=(
MASS_UNIT()
NAMED_UNIT(*)
SI_UNIT(.KILO.,.GRAM.)
);
#6347=DERIVED_UNIT((#6260,#6261));
#6348=DERIVED_UNIT((#6262,#6263));
#6349=DERIVED_UNIT((#6264,#6265));
#6350=DERIVED_UNIT((#6266,#6267));
#6351=DERIVED_UNIT((#6268,#6269));
#6352=DERIVED_UNIT((#6270,#6271));
#6353=DERIVED_UNIT((#6272,#6273));
#6354=DERIVED_UNIT((#6274,#6275));
#6355=DERIVED_UNIT((#6276,#6277));
#6356=DERIVED_UNIT((#6278,#6279));
#6357=DERIVED_UNIT((#6280,#6281));
#6358=DERIVED_UNIT((#6282,#6283));
#6359=DERIVED_UNIT((#6284,#6285));
#6360=DERIVED_UNIT((#6286,#6287));
#6361=DERIVED_UNIT((#6288,#6289));
#6362=DERIVED_UNIT((#6290,#6291));
#6363=DERIVED_UNIT((#6292,#6293));
#6364=DERIVED_UNIT((#6294,#6295));
#6365=DERIVED_UNIT((#6296,#6297));
#6366=DERIVED_UNIT((#6298,#6299));
#6367=DERIVED_UNIT((#6300,#6301));
#6368=DERIVED_UNIT((#6302,#6303));
#6369=DERIVED_UNIT((#6304,#6305));
#6370=DERIVED_UNIT((#6306,#6307));
#6371=DERIVED_UNIT((#6308,#6309));
#6372=DERIVED_UNIT((#6310,#6311));
#6373=DERIVED_UNIT((#6312,#6313));
#6374=DERIVED_UNIT((#6314,#6315));
#6375=DERIVED_UNIT((#6316,#6317));
#6376=DERIVED_UNIT((#6318,#6319));
#6377=DERIVED_UNIT((#6320,#6321));
#6378=DERIVED_UNIT((#6322,#6323));
#6379=DERIVED_UNIT((#6324,#6325));
#6380=DERIVED_UNIT((#6326,#6327));
#6381=DERIVED_UNIT((#6328,#6329));
#6382=DERIVED_UNIT((#6330,#6331));
#6383=DERIVED_UNIT((#6332,#6333));
#6384=DERIVED_UNIT((#6334,#6335));
#6385=DERIVED_UNIT((#6336,#6337));
#6386=DERIVED_UNIT((#6338,#6339));
#6387=DERIVED_UNIT((#6340,#6341));
#6388=DERIVED_UNIT((#6342,#6343));
#6389=DERIVED_UNIT((#6344,#6345));
#6390=MEASURE_REPRESENTATION_ITEM('density measure',
POSITIVE_RATIO_MEASURE(7850.),#6347);
#6391=MEASURE_REPRESENTATION_ITEM('density measure',
POSITIVE_RATIO_MEASURE(7850.),#6348);
#6392=MEASURE_REPRESENTATION_ITEM('density measure',
POSITIVE_RATIO_MEASURE(7850.),#6349);
#6393=MEASURE_REPRESENTATION_ITEM('density measure',
POSITIVE_RATIO_MEASURE(7850.),#6350);
#6394=MEASURE_REPRESENTATION_ITEM('density measure',
POSITIVE_RATIO_MEASURE(7850.),#6351);
#6395=MEASURE_REPRESENTATION_ITEM('density measure',
POSITIVE_RATIO_MEASURE(7850.),#6352);
#6396=MEASURE_REPRESENTATION_ITEM('density measure',
POSITIVE_RATIO_MEASURE(7850.),#6353);
#6397=MEASURE_REPRESENTATION_ITEM('density measure',
POSITIVE_RATIO_MEASURE(7850.),#6354);
#6398=MEASURE_REPRESENTATION_ITEM('density measure',
POSITIVE_RATIO_MEASURE(7850.),#6355);
#6399=MEASURE_REPRESENTATION_ITEM('density measure',
POSITIVE_RATIO_MEASURE(7850.),#6356);
#6400=MEASURE_REPRESENTATION_ITEM('density measure',
POSITIVE_RATIO_MEASURE(7850.),#6357);
#6401=MEASURE_REPRESENTATION_ITEM('density measure',
POSITIVE_RATIO_MEASURE(7850.),#6358);
#6402=MEASURE_REPRESENTATION_ITEM('density measure',
POSITIVE_RATIO_MEASURE(7850.),#6359);
#6403=MEASURE_REPRESENTATION_ITEM('density measure',
POSITIVE_RATIO_MEASURE(7850.),#6360);
#6404=MEASURE_REPRESENTATION_ITEM('density measure',
POSITIVE_RATIO_MEASURE(7850.),#6361);
#6405=MEASURE_REPRESENTATION_ITEM('density measure',
POSITIVE_RATIO_MEASURE(7850.),#6362);
#6406=MEASURE_REPRESENTATION_ITEM('density measure',
POSITIVE_RATIO_MEASURE(7850.),#6363);
#6407=MEASURE_REPRESENTATION_ITEM('density measure',
POSITIVE_RATIO_MEASURE(7850.),#6364);
#6408=MEASURE_REPRESENTATION_ITEM('density measure',
POSITIVE_RATIO_MEASURE(7850.),#6365);
#6409=MEASURE_REPRESENTATION_ITEM('density measure',
POSITIVE_RATIO_MEASURE(7850.),#6366);
#6410=MEASURE_REPRESENTATION_ITEM('density measure',
POSITIVE_RATIO_MEASURE(7850.),#6367);
#6411=MEASURE_REPRESENTATION_ITEM('density measure',
POSITIVE_RATIO_MEASURE(7850.),#6368);
#6412=MEASURE_REPRESENTATION_ITEM('density measure',
POSITIVE_RATIO_MEASURE(7850.),#6369);
#6413=MEASURE_REPRESENTATION_ITEM('density measure',
POSITIVE_RATIO_MEASURE(7850.),#6370);
#6414=MEASURE_REPRESENTATION_ITEM('density measure',
POSITIVE_RATIO_MEASURE(7850.),#6371);
#6415=MEASURE_REPRESENTATION_ITEM('density measure',
POSITIVE_RATIO_MEASURE(7850.),#6372);
#6416=MEASURE_REPRESENTATION_ITEM('density measure',
POSITIVE_RATIO_MEASURE(7850.),#6373);
#6417=MEASURE_REPRESENTATION_ITEM('density measure',
POSITIVE_RATIO_MEASURE(7850.),#6374);
#6418=MEASURE_REPRESENTATION_ITEM('density measure',
POSITIVE_RATIO_MEASURE(7850.),#6375);
#6419=MEASURE_REPRESENTATION_ITEM('density measure',
POSITIVE_RATIO_MEASURE(7850.),#6376);
#6420=MEASURE_REPRESENTATION_ITEM('density measure',
POSITIVE_RATIO_MEASURE(7850.),#6377);
#6421=MEASURE_REPRESENTATION_ITEM('density measure',
POSITIVE_RATIO_MEASURE(7850.),#6378);
#6422=MEASURE_REPRESENTATION_ITEM('density measure',
POSITIVE_RATIO_MEASURE(7850.),#6379);
#6423=MEASURE_REPRESENTATION_ITEM('density measure',
POSITIVE_RATIO_MEASURE(7850.),#6380);
#6424=MEASURE_REPRESENTATION_ITEM('density measure',
POSITIVE_RATIO_MEASURE(7850.),#6381);
#6425=MEASURE_REPRESENTATION_ITEM('density measure',
POSITIVE_RATIO_MEASURE(7850.),#6382);
#6426=MEASURE_REPRESENTATION_ITEM('density measure',
POSITIVE_RATIO_MEASURE(7850.),#6383);
#6427=MEASURE_REPRESENTATION_ITEM('density measure',
POSITIVE_RATIO_MEASURE(7850.),#6384);
#6428=MEASURE_REPRESENTATION_ITEM('density measure',
POSITIVE_RATIO_MEASURE(7850.),#6385);
#6429=MEASURE_REPRESENTATION_ITEM('density measure',
POSITIVE_RATIO_MEASURE(7850.),#6386);
#6430=MEASURE_REPRESENTATION_ITEM('density measure',
POSITIVE_RATIO_MEASURE(7850.),#6387);
#6431=MEASURE_REPRESENTATION_ITEM('density measure',
POSITIVE_RATIO_MEASURE(7850.),#6388);
#6432=MEASURE_REPRESENTATION_ITEM('density measure',
POSITIVE_RATIO_MEASURE(7850.),#6389);
#6433=PROPERTY_DEFINITION_REPRESENTATION(#6648,#6519);
#6434=PROPERTY_DEFINITION_REPRESENTATION(#6649,#6520);
#6435=PROPERTY_DEFINITION_REPRESENTATION(#6650,#6521);
#6436=PROPERTY_DEFINITION_REPRESENTATION(#6651,#6522);
#6437=PROPERTY_DEFINITION_REPRESENTATION(#6652,#6523);
#6438=PROPERTY_DEFINITION_REPRESENTATION(#6653,#6524);
#6439=PROPERTY_DEFINITION_REPRESENTATION(#6654,#6525);
#6440=PROPERTY_DEFINITION_REPRESENTATION(#6655,#6526);
#6441=PROPERTY_DEFINITION_REPRESENTATION(#6656,#6527);
#6442=PROPERTY_DEFINITION_REPRESENTATION(#6657,#6528);
#6443=PROPERTY_DEFINITION_REPRESENTATION(#6658,#6529);
#6444=PROPERTY_DEFINITION_REPRESENTATION(#6659,#6530);
#6445=PROPERTY_DEFINITION_REPRESENTATION(#6660,#6531);
#6446=PROPERTY_DEFINITION_REPRESENTATION(#6661,#6532);
#6447=PROPERTY_DEFINITION_REPRESENTATION(#6662,#6533);
#6448=PROPERTY_DEFINITION_REPRESENTATION(#6663,#6534);
#6449=PROPERTY_DEFINITION_REPRESENTATION(#6664,#6535);
#6450=PROPERTY_DEFINITION_REPRESENTATION(#6665,#6536);
#6451=PROPERTY_DEFINITION_REPRESENTATION(#6666,#6537);
#6452=PROPERTY_DEFINITION_REPRESENTATION(#6667,#6538);
#6453=PROPERTY_DEFINITION_REPRESENTATION(#6668,#6539);
#6454=PROPERTY_DEFINITION_REPRESENTATION(#6669,#6540);
#6455=PROPERTY_DEFINITION_REPRESENTATION(#6670,#6541);
#6456=PROPERTY_DEFINITION_REPRESENTATION(#6671,#6542);
#6457=PROPERTY_DEFINITION_REPRESENTATION(#6672,#6543);
#6458=PROPERTY_DEFINITION_REPRESENTATION(#6673,#6544);
#6459=PROPERTY_DEFINITION_REPRESENTATION(#6674,#6545);
#6460=PROPERTY_DEFINITION_REPRESENTATION(#6675,#6546);
#6461=PROPERTY_DEFINITION_REPRESENTATION(#6676,#6547);
#6462=PROPERTY_DEFINITION_REPRESENTATION(#6677,#6548);
#6463=PROPERTY_DEFINITION_REPRESENTATION(#6678,#6549);
#6464=PROPERTY_DEFINITION_REPRESENTATION(#6679,#6550);
#6465=PROPERTY_DEFINITION_REPRESENTATION(#6680,#6551);
#6466=PROPERTY_DEFINITION_REPRESENTATION(#6681,#6552);
#6467=PROPERTY_DEFINITION_REPRESENTATION(#6682,#6553);
#6468=PROPERTY_DEFINITION_REPRESENTATION(#6683,#6554);
#6469=PROPERTY_DEFINITION_REPRESENTATION(#6684,#6555);
#6470=PROPERTY_DEFINITION_REPRESENTATION(#6685,#6556);
#6471=PROPERTY_DEFINITION_REPRESENTATION(#6686,#6557);
#6472=PROPERTY_DEFINITION_REPRESENTATION(#6687,#6558);
#6473=PROPERTY_DEFINITION_REPRESENTATION(#6688,#6559);
#6474=PROPERTY_DEFINITION_REPRESENTATION(#6689,#6560);
#6475=PROPERTY_DEFINITION_REPRESENTATION(#6690,#6561);
#6476=PROPERTY_DEFINITION_REPRESENTATION(#6691,#6562);
#6477=PROPERTY_DEFINITION_REPRESENTATION(#6692,#6563);
#6478=PROPERTY_DEFINITION_REPRESENTATION(#6693,#6564);
#6479=PROPERTY_DEFINITION_REPRESENTATION(#6694,#6565);
#6480=PROPERTY_DEFINITION_REPRESENTATION(#6695,#6566);
#6481=PROPERTY_DEFINITION_REPRESENTATION(#6696,#6567);
#6482=PROPERTY_DEFINITION_REPRESENTATION(#6697,#6568);
#6483=PROPERTY_DEFINITION_REPRESENTATION(#6698,#6569);
#6484=PROPERTY_DEFINITION_REPRESENTATION(#6699,#6570);
#6485=PROPERTY_DEFINITION_REPRESENTATION(#6700,#6571);
#6486=PROPERTY_DEFINITION_REPRESENTATION(#6701,#6572);
#6487=PROPERTY_DEFINITION_REPRESENTATION(#6702,#6573);
#6488=PROPERTY_DEFINITION_REPRESENTATION(#6703,#6574);
#6489=PROPERTY_DEFINITION_REPRESENTATION(#6704,#6575);
#6490=PROPERTY_DEFINITION_REPRESENTATION(#6705,#6576);
#6491=PROPERTY_DEFINITION_REPRESENTATION(#6706,#6577);
#6492=PROPERTY_DEFINITION_REPRESENTATION(#6707,#6578);
#6493=PROPERTY_DEFINITION_REPRESENTATION(#6708,#6579);
#6494=PROPERTY_DEFINITION_REPRESENTATION(#6709,#6580);
#6495=PROPERTY_DEFINITION_REPRESENTATION(#6710,#6581);
#6496=PROPERTY_DEFINITION_REPRESENTATION(#6711,#6582);
#6497=PROPERTY_DEFINITION_REPRESENTATION(#6712,#6583);
#6498=PROPERTY_DEFINITION_REPRESENTATION(#6713,#6584);
#6499=PROPERTY_DEFINITION_REPRESENTATION(#6714,#6585);
#6500=PROPERTY_DEFINITION_REPRESENTATION(#6715,#6586);
#6501=PROPERTY_DEFINITION_REPRESENTATION(#6716,#6587);
#6502=PROPERTY_DEFINITION_REPRESENTATION(#6717,#6588);
#6503=PROPERTY_DEFINITION_REPRESENTATION(#6718,#6589);
#6504=PROPERTY_DEFINITION_REPRESENTATION(#6719,#6590);
#6505=PROPERTY_DEFINITION_REPRESENTATION(#6720,#6591);
#6506=PROPERTY_DEFINITION_REPRESENTATION(#6721,#6592);
#6507=PROPERTY_DEFINITION_REPRESENTATION(#6722,#6593);
#6508=PROPERTY_DEFINITION_REPRESENTATION(#6723,#6594);
#6509=PROPERTY_DEFINITION_REPRESENTATION(#6724,#6595);
#6510=PROPERTY_DEFINITION_REPRESENTATION(#6725,#6596);
#6511=PROPERTY_DEFINITION_REPRESENTATION(#6726,#6597);
#6512=PROPERTY_DEFINITION_REPRESENTATION(#6727,#6598);
#6513=PROPERTY_DEFINITION_REPRESENTATION(#6728,#6599);
#6514=PROPERTY_DEFINITION_REPRESENTATION(#6729,#6600);
#6515=PROPERTY_DEFINITION_REPRESENTATION(#6730,#6601);
#6516=PROPERTY_DEFINITION_REPRESENTATION(#6731,#6602);
#6517=PROPERTY_DEFINITION_REPRESENTATION(#6732,#6603);
#6518=PROPERTY_DEFINITION_REPRESENTATION(#6733,#6604);
#6519=REPRESENTATION('material name',(#6605),#11702);
#6520=REPRESENTATION('density',(#6390),#11702);
#6521=REPRESENTATION('material name',(#6606),#11703);
#6522=REPRESENTATION('density',(#6391),#11703);
#6523=REPRESENTATION('material name',(#6607),#11704);
#6524=REPRESENTATION('density',(#6392),#11704);
#6525=REPRESENTATION('material name',(#6608),#11705);
#6526=REPRESENTATION('density',(#6393),#11705);
#6527=REPRESENTATION('material name',(#6609),#11706);
#6528=REPRESENTATION('density',(#6394),#11706);
#6529=REPRESENTATION('material name',(#6610),#11707);
#6530=REPRESENTATION('density',(#6395),#11707);
#6531=REPRESENTATION('material name',(#6611),#11708);
#6532=REPRESENTATION('density',(#6396),#11708);
#6533=REPRESENTATION('material name',(#6612),#11709);
#6534=REPRESENTATION('density',(#6397),#11709);
#6535=REPRESENTATION('material name',(#6613),#11710);
#6536=REPRESENTATION('density',(#6398),#11710);
#6537=REPRESENTATION('material name',(#6614),#11711);
#6538=REPRESENTATION('density',(#6399),#11711);
#6539=REPRESENTATION('material name',(#6615),#11712);
#6540=REPRESENTATION('density',(#6400),#11712);
#6541=REPRESENTATION('material name',(#6616),#11713);
#6542=REPRESENTATION('density',(#6401),#11713);
#6543=REPRESENTATION('material name',(#6617),#11714);
#6544=REPRESENTATION('density',(#6402),#11714);
#6545=REPRESENTATION('material name',(#6618),#11715);
#6546=REPRESENTATION('density',(#6403),#11715);
#6547=REPRESENTATION('material name',(#6619),#11716);
#6548=REPRESENTATION('density',(#6404),#11716);
#6549=REPRESENTATION('material name',(#6620),#11717);
#6550=REPRESENTATION('density',(#6405),#11717);
#6551=REPRESENTATION('material name',(#6621),#11718);
#6552=REPRESENTATION('density',(#6406),#11718);
#6553=REPRESENTATION('material name',(#6622),#11719);
#6554=REPRESENTATION('density',(#6407),#11719);
#6555=REPRESENTATION('material name',(#6623),#11720);
#6556=REPRESENTATION('density',(#6408),#11720);
#6557=REPRESENTATION('material name',(#6624),#11721);
#6558=REPRESENTATION('density',(#6409),#11721);
#6559=REPRESENTATION('material name',(#6625),#11722);
#6560=REPRESENTATION('density',(#6410),#11722);
#6561=REPRESENTATION('material name',(#6626),#11723);
#6562=REPRESENTATION('density',(#6411),#11723);
#6563=REPRESENTATION('material name',(#6627),#11724);
#6564=REPRESENTATION('density',(#6412),#11724);
#6565=REPRESENTATION('material name',(#6628),#11725);
#6566=REPRESENTATION('density',(#6413),#11725);
#6567=REPRESENTATION('material name',(#6629),#11726);
#6568=REPRESENTATION('density',(#6414),#11726);
#6569=REPRESENTATION('material name',(#6630),#11727);
#6570=REPRESENTATION('density',(#6415),#11727);
#6571=REPRESENTATION('material name',(#6631),#11728);
#6572=REPRESENTATION('density',(#6416),#11728);
#6573=REPRESENTATION('material name',(#6632),#11729);
#6574=REPRESENTATION('density',(#6417),#11729);
#6575=REPRESENTATION('material name',(#6633),#11730);
#6576=REPRESENTATION('density',(#6418),#11730);
#6577=REPRESENTATION('material name',(#6634),#11731);
#6578=REPRESENTATION('density',(#6419),#11731);
#6579=REPRESENTATION('material name',(#6635),#11732);
#6580=REPRESENTATION('density',(#6420),#11732);
#6581=REPRESENTATION('material name',(#6636),#11733);
#6582=REPRESENTATION('density',(#6421),#11733);
#6583=REPRESENTATION('material name',(#6637),#11734);
#6584=REPRESENTATION('density',(#6422),#11734);
#6585=REPRESENTATION('material name',(#6638),#11735);
#6586=REPRESENTATION('density',(#6423),#11735);
#6587=REPRESENTATION('material name',(#6639),#11737);
#6588=REPRESENTATION('density',(#6424),#11737);
#6589=REPRESENTATION('material name',(#6640),#11740);
#6590=REPRESENTATION('density',(#6425),#11740);
#6591=REPRESENTATION('material name',(#6641),#11741);
#6592=REPRESENTATION('density',(#6426),#11741);
#6593=REPRESENTATION('material name',(#6642),#11742);
#6594=REPRESENTATION('density',(#6427),#11742);
#6595=REPRESENTATION('material name',(#6643),#11743);
#6596=REPRESENTATION('density',(#6428),#11743);
#6597=REPRESENTATION('material name',(#6644),#11744);
#6598=REPRESENTATION('density',(#6429),#11744);
#6599=REPRESENTATION('material name',(#6645),#11745);
#6600=REPRESENTATION('density',(#6430),#11745);
#6601=REPRESENTATION('material name',(#6646),#11746);
#6602=REPRESENTATION('density',(#6431),#11746);
#6603=REPRESENTATION('material name',(#6647),#11747);
#6604=REPRESENTATION('density',(#6432),#11747);
#6605=DESCRIPTIVE_REPRESENTATION_ITEM('Steel','Steel');
#6606=DESCRIPTIVE_REPRESENTATION_ITEM('Steel','Steel');
#6607=DESCRIPTIVE_REPRESENTATION_ITEM('Steel','Steel');
#6608=DESCRIPTIVE_REPRESENTATION_ITEM('Steel','Steel');
#6609=DESCRIPTIVE_REPRESENTATION_ITEM('Steel','Steel');
#6610=DESCRIPTIVE_REPRESENTATION_ITEM('Steel','Steel');
#6611=DESCRIPTIVE_REPRESENTATION_ITEM('Steel','Steel');
#6612=DESCRIPTIVE_REPRESENTATION_ITEM('Steel','Steel');
#6613=DESCRIPTIVE_REPRESENTATION_ITEM('Steel','Steel');
#6614=DESCRIPTIVE_REPRESENTATION_ITEM('Steel','Steel');
#6615=DESCRIPTIVE_REPRESENTATION_ITEM('Steel','Steel');
#6616=DESCRIPTIVE_REPRESENTATION_ITEM('Steel','Steel');
#6617=DESCRIPTIVE_REPRESENTATION_ITEM('Steel','Steel');
#6618=DESCRIPTIVE_REPRESENTATION_ITEM('Steel','Steel');
#6619=DESCRIPTIVE_REPRESENTATION_ITEM('Steel','Steel');
#6620=DESCRIPTIVE_REPRESENTATION_ITEM('Steel','Steel');
#6621=DESCRIPTIVE_REPRESENTATION_ITEM('Steel','Steel');
#6622=DESCRIPTIVE_REPRESENTATION_ITEM('Steel','Steel');
#6623=DESCRIPTIVE_REPRESENTATION_ITEM('Steel','Steel');
#6624=DESCRIPTIVE_REPRESENTATION_ITEM('Steel','Steel');
#6625=DESCRIPTIVE_REPRESENTATION_ITEM('Steel','Steel');
#6626=DESCRIPTIVE_REPRESENTATION_ITEM('Steel','Steel');
#6627=DESCRIPTIVE_REPRESENTATION_ITEM('Steel','Steel');
#6628=DESCRIPTIVE_REPRESENTATION_ITEM('Steel','Steel');
#6629=DESCRIPTIVE_REPRESENTATION_ITEM('Steel','Steel');
#6630=DESCRIPTIVE_REPRESENTATION_ITEM('Steel','Steel');
#6631=DESCRIPTIVE_REPRESENTATION_ITEM('Steel','Steel');
#6632=DESCRIPTIVE_REPRESENTATION_ITEM('Steel','Steel');
#6633=DESCRIPTIVE_REPRESENTATION_ITEM('Steel','Steel');
#6634=DESCRIPTIVE_REPRESENTATION_ITEM('Steel','Steel');
#6635=DESCRIPTIVE_REPRESENTATION_ITEM('Steel','Steel');
#6636=DESCRIPTIVE_REPRESENTATION_ITEM('Steel','Steel');
#6637=DESCRIPTIVE_REPRESENTATION_ITEM('Steel','Steel');
#6638=DESCRIPTIVE_REPRESENTATION_ITEM('Steel','Steel');
#6639=DESCRIPTIVE_REPRESENTATION_ITEM('Steel','Steel');
#6640=DESCRIPTIVE_REPRESENTATION_ITEM('Steel','Steel');
#6641=DESCRIPTIVE_REPRESENTATION_ITEM('Steel','Steel');
#6642=DESCRIPTIVE_REPRESENTATION_ITEM('Steel','Steel');
#6643=DESCRIPTIVE_REPRESENTATION_ITEM('Steel','Steel');
#6644=DESCRIPTIVE_REPRESENTATION_ITEM('Steel','Steel');
#6645=DESCRIPTIVE_REPRESENTATION_ITEM('Steel','Steel');
#6646=DESCRIPTIVE_REPRESENTATION_ITEM('Steel','Steel');
#6647=DESCRIPTIVE_REPRESENTATION_ITEM('Steel','Steel');
#6648=PROPERTY_DEFINITION('material property','material name',#11975);
#6649=PROPERTY_DEFINITION('material property','density of part',#11975);
#6650=PROPERTY_DEFINITION('material property','material name',#11976);
#6651=PROPERTY_DEFINITION('material property','density of part',#11976);
#6652=PROPERTY_DEFINITION('material property','material name',#11977);
#6653=PROPERTY_DEFINITION('material property','density of part',#11977);
#6654=PROPERTY_DEFINITION('material property','material name',#11978);
#6655=PROPERTY_DEFINITION('material property','density of part',#11978);
#6656=PROPERTY_DEFINITION('material property','material name',#11979);
#6657=PROPERTY_DEFINITION('material property','density of part',#11979);
#6658=PROPERTY_DEFINITION('material property','material name',#11980);
#6659=PROPERTY_DEFINITION('material property','density of part',#11980);
#6660=PROPERTY_DEFINITION('material property','material name',#11981);
#6661=PROPERTY_DEFINITION('material property','density of part',#11981);
#6662=PROPERTY_DEFINITION('material property','material name',#11982);
#6663=PROPERTY_DEFINITION('material property','density of part',#11982);
#6664=PROPERTY_DEFINITION('material property','material name',#11983);
#6665=PROPERTY_DEFINITION('material property','density of part',#11983);
#6666=PROPERTY_DEFINITION('material property','material name',#11984);
#6667=PROPERTY_DEFINITION('material property','density of part',#11984);
#6668=PROPERTY_DEFINITION('material property','material name',#11985);
#6669=PROPERTY_DEFINITION('material property','density of part',#11985);
#6670=PROPERTY_DEFINITION('material property','material name',#11986);
#6671=PROPERTY_DEFINITION('material property','density of part',#11986);
#6672=PROPERTY_DEFINITION('material property','material name',#11987);
#6673=PROPERTY_DEFINITION('material property','density of part',#11987);
#6674=PROPERTY_DEFINITION('material property','material name',#11988);
#6675=PROPERTY_DEFINITION('material property','density of part',#11988);
#6676=PROPERTY_DEFINITION('material property','material name',#11989);
#6677=PROPERTY_DEFINITION('material property','density of part',#11989);
#6678=PROPERTY_DEFINITION('material property','material name',#11990);
#6679=PROPERTY_DEFINITION('material property','density of part',#11990);
#6680=PROPERTY_DEFINITION('material property','material name',#11991);
#6681=PROPERTY_DEFINITION('material property','density of part',#11991);
#6682=PROPERTY_DEFINITION('material property','material name',#11992);
#6683=PROPERTY_DEFINITION('material property','density of part',#11992);
#6684=PROPERTY_DEFINITION('material property','material name',#11993);
#6685=PROPERTY_DEFINITION('material property','density of part',#11993);
#6686=PROPERTY_DEFINITION('material property','material name',#11994);
#6687=PROPERTY_DEFINITION('material property','density of part',#11994);
#6688=PROPERTY_DEFINITION('material property','material name',#11995);
#6689=PROPERTY_DEFINITION('material property','density of part',#11995);
#6690=PROPERTY_DEFINITION('material property','material name',#11996);
#6691=PROPERTY_DEFINITION('material property','density of part',#11996);
#6692=PROPERTY_DEFINITION('material property','material name',#11997);
#6693=PROPERTY_DEFINITION('material property','density of part',#11997);
#6694=PROPERTY_DEFINITION('material property','material name',#11998);
#6695=PROPERTY_DEFINITION('material property','density of part',#11998);
#6696=PROPERTY_DEFINITION('material property','material name',#11999);
#6697=PROPERTY_DEFINITION('material property','density of part',#11999);
#6698=PROPERTY_DEFINITION('material property','material name',#12000);
#6699=PROPERTY_DEFINITION('material property','density of part',#12000);
#6700=PROPERTY_DEFINITION('material property','material name',#12001);
#6701=PROPERTY_DEFINITION('material property','density of part',#12001);
#6702=PROPERTY_DEFINITION('material property','material name',#12002);
#6703=PROPERTY_DEFINITION('material property','density of part',#12002);
#6704=PROPERTY_DEFINITION('material property','material name',#12003);
#6705=PROPERTY_DEFINITION('material property','density of part',#12003);
#6706=PROPERTY_DEFINITION('material property','material name',#12004);
#6707=PROPERTY_DEFINITION('material property','density of part',#12004);
#6708=PROPERTY_DEFINITION('material property','material name',#12005);
#6709=PROPERTY_DEFINITION('material property','density of part',#12005);
#6710=PROPERTY_DEFINITION('material property','material name',#12006);
#6711=PROPERTY_DEFINITION('material property','density of part',#12006);
#6712=PROPERTY_DEFINITION('material property','material name',#12007);
#6713=PROPERTY_DEFINITION('material property','density of part',#12007);
#6714=PROPERTY_DEFINITION('material property','material name',#12008);
#6715=PROPERTY_DEFINITION('material property','density of part',#12008);
#6716=PROPERTY_DEFINITION('material property','material name',#12010);
#6717=PROPERTY_DEFINITION('material property','density of part',#12010);
#6718=PROPERTY_DEFINITION('material property','material name',#12013);
#6719=PROPERTY_DEFINITION('material property','density of part',#12013);
#6720=PROPERTY_DEFINITION('material property','material name',#12014);
#6721=PROPERTY_DEFINITION('material property','density of part',#12014);
#6722=PROPERTY_DEFINITION('material property','material name',#12015);
#6723=PROPERTY_DEFINITION('material property','density of part',#12015);
#6724=PROPERTY_DEFINITION('material property','material name',#12016);
#6725=PROPERTY_DEFINITION('material property','density of part',#12016);
#6726=PROPERTY_DEFINITION('material property','material name',#12017);
#6727=PROPERTY_DEFINITION('material property','density of part',#12017);
#6728=PROPERTY_DEFINITION('material property','material name',#12018);
#6729=PROPERTY_DEFINITION('material property','density of part',#12018);
#6730=PROPERTY_DEFINITION('material property','material name',#12019);
#6731=PROPERTY_DEFINITION('material property','density of part',#12019);
#6732=PROPERTY_DEFINITION('material property','material name',#12020);
#6733=PROPERTY_DEFINITION('material property','density of part',#12020);
#6734=AXIS2_PLACEMENT_3D('',#9475,#7492,#7493);
#6735=AXIS2_PLACEMENT_3D('',#9476,#7494,#7495);
#6736=AXIS2_PLACEMENT_3D('',#9477,#7496,#7497);
#6737=AXIS2_PLACEMENT_3D('',#9478,#7498,#7499);
#6738=AXIS2_PLACEMENT_3D('',#9487,#7504,#7505);
#6739=AXIS2_PLACEMENT_3D('',#9493,#7509,#7510);
#6740=AXIS2_PLACEMENT_3D('',#9499,#7514,#7515);
#6741=AXIS2_PLACEMENT_3D('',#9505,#7519,#7520);
#6742=AXIS2_PLACEMENT_3D('',#9511,#7524,#7525);
#6743=AXIS2_PLACEMENT_3D('',#9517,#7529,#7530);
#6744=AXIS2_PLACEMENT_3D('',#9523,#7534,#7535);
#6745=AXIS2_PLACEMENT_3D('',#9529,#7539,#7540);
#6746=AXIS2_PLACEMENT_3D('',#9535,#7544,#7545);
#6747=AXIS2_PLACEMENT_3D('',#9544,#7550,#7551);
#6748=AXIS2_PLACEMENT_3D('',#9550,#7555,#7556);
#6749=AXIS2_PLACEMENT_3D('',#9556,#7560,#7561);
#6750=AXIS2_PLACEMENT_3D('',#9562,#7565,#7566);
#6751=AXIS2_PLACEMENT_3D('',#9568,#7570,#7571);
#6752=AXIS2_PLACEMENT_3D('',#9574,#7575,#7576);
#6753=AXIS2_PLACEMENT_3D('',#9580,#7580,#7581);
#6754=AXIS2_PLACEMENT_3D('',#9586,#7585,#7586);
#6755=AXIS2_PLACEMENT_3D('',#9592,#7590,#7591);
#6756=AXIS2_PLACEMENT_3D('',#9601,#7596,#7597);
#6757=AXIS2_PLACEMENT_3D('',#9607,#7601,#7602);
#6758=AXIS2_PLACEMENT_3D('',#9613,#7606,#7607);
#6759=AXIS2_PLACEMENT_3D('',#9619,#7611,#7612);
#6760=AXIS2_PLACEMENT_3D('',#9625,#7616,#7617);
#6761=AXIS2_PLACEMENT_3D('',#9631,#7621,#7622);
#6762=AXIS2_PLACEMENT_3D('',#9637,#7626,#7627);
#6763=AXIS2_PLACEMENT_3D('',#9643,#7631,#7632);
#6764=AXIS2_PLACEMENT_3D('',#9649,#7636,#7637);
#6765=AXIS2_PLACEMENT_3D('',#9658,#7642,#7643);
#6766=AXIS2_PLACEMENT_3D('',#9664,#7647,#7648);
#6767=AXIS2_PLACEMENT_3D('',#9670,#7652,#7653);
#6768=AXIS2_PLACEMENT_3D('',#9676,#7657,#7658);
#6769=AXIS2_PLACEMENT_3D('',#9682,#7662,#7663);
#6770=AXIS2_PLACEMENT_3D('',#9688,#7667,#7668);
#6771=AXIS2_PLACEMENT_3D('',#9694,#7672,#7673);
#6772=AXIS2_PLACEMENT_3D('',#9700,#7677,#7678);
#6773=AXIS2_PLACEMENT_3D('',#9706,#7682,#7683);
#6774=AXIS2_PLACEMENT_3D('',#9708,#7684,#7685);
#6775=AXIS2_PLACEMENT_3D('',#9711,#7687,#7688);
#6776=AXIS2_PLACEMENT_3D('',#9712,#7689,#7690);
#6777=AXIS2_PLACEMENT_3D('',#9718,#7694,#7695);
#6778=AXIS2_PLACEMENT_3D('',#9724,#7699,#7700);
#6779=AXIS2_PLACEMENT_3D('',#9727,#7703,#7704);
#6780=AXIS2_PLACEMENT_3D('',#9733,#7708,#7709);
#6781=AXIS2_PLACEMENT_3D('',#9736,#7712,#7713);
#6782=AXIS2_PLACEMENT_3D('',#9742,#7717,#7718);
#6783=AXIS2_PLACEMENT_3D('',#9745,#7721,#7722);
#6784=AXIS2_PLACEMENT_3D('',#9748,#7725,#7726);
#6785=AXIS2_PLACEMENT_3D('',#9749,#7727,#7728);
#6786=AXIS2_PLACEMENT_3D('',#9750,#7729,#7730);
#6787=AXIS2_PLACEMENT_3D('',#9751,#7731,#7732);
#6788=AXIS2_PLACEMENT_3D('',#9753,#7733,#7734);
#6789=AXIS2_PLACEMENT_3D('',#9756,#7736,#7737);
#6790=AXIS2_PLACEMENT_3D('',#9757,#7738,#7739);
#6791=AXIS2_PLACEMENT_3D('',#9759,#7740,#7741);
#6792=AXIS2_PLACEMENT_3D('',#9762,#7743,#7744);
#6793=AXIS2_PLACEMENT_3D('',#9763,#7745,#7746);
#6794=AXIS2_PLACEMENT_3D('',#9765,#7747,#7748);
#6795=AXIS2_PLACEMENT_3D('',#9768,#7750,#7751);
#6796=AXIS2_PLACEMENT_3D('',#9769,#7752,#7753);
#6797=AXIS2_PLACEMENT_3D('',#9771,#7754,#7755);
#6798=AXIS2_PLACEMENT_3D('',#9774,#7757,#7758);
#6799=AXIS2_PLACEMENT_3D('',#9775,#7759,#7760);
#6800=AXIS2_PLACEMENT_3D('',#9777,#7761,#7762);
#6801=AXIS2_PLACEMENT_3D('',#9780,#7764,#7765);
#6802=AXIS2_PLACEMENT_3D('',#9781,#7766,#7767);
#6803=AXIS2_PLACEMENT_3D('',#9783,#7768,#7769);
#6804=AXIS2_PLACEMENT_3D('',#9786,#7771,#7772);
#6805=AXIS2_PLACEMENT_3D('',#9787,#7773,#7774);
#6806=AXIS2_PLACEMENT_3D('',#9789,#7775,#7776);
#6807=AXIS2_PLACEMENT_3D('',#9792,#7778,#7779);
#6808=AXIS2_PLACEMENT_3D('',#9793,#7780,#7781);
#6809=AXIS2_PLACEMENT_3D('',#9795,#7782,#7783);
#6810=AXIS2_PLACEMENT_3D('',#9798,#7785,#7786);
#6811=AXIS2_PLACEMENT_3D('',#9799,#7787,#7788);
#6812=AXIS2_PLACEMENT_3D('',#9801,#7789,#7790);
#6813=AXIS2_PLACEMENT_3D('',#9804,#7792,#7793);
#6814=AXIS2_PLACEMENT_3D('',#9805,#7794,#7795);
#6815=AXIS2_PLACEMENT_3D('',#9807,#7796,#7797);
#6816=AXIS2_PLACEMENT_3D('',#9810,#7799,#7800);
#6817=AXIS2_PLACEMENT_3D('',#9811,#7801,#7802);
#6818=AXIS2_PLACEMENT_3D('',#9813,#7803,#7804);
#6819=AXIS2_PLACEMENT_3D('',#9816,#7806,#7807);
#6820=AXIS2_PLACEMENT_3D('',#9817,#7808,#7809);
#6821=AXIS2_PLACEMENT_3D('',#9819,#7810,#7811);
#6822=AXIS2_PLACEMENT_3D('',#9822,#7813,#7814);
#6823=AXIS2_PLACEMENT_3D('',#9823,#7815,#7816);
#6824=AXIS2_PLACEMENT_3D('',#9832,#7821,#7822);
#6825=AXIS2_PLACEMENT_3D('',#9838,#7826,#7827);
#6826=AXIS2_PLACEMENT_3D('',#9844,#7831,#7832);
#6827=AXIS2_PLACEMENT_3D('',#9847,#7835,#7836);
#6828=AXIS2_PLACEMENT_3D('',#9848,#7837,#7838);
#6829=AXIS2_PLACEMENT_3D('',#9849,#7839,#7840);
#6830=AXIS2_PLACEMENT_3D('',#9850,#7841,#7842);
#6831=AXIS2_PLACEMENT_3D('',#9859,#7847,#7848);
#6832=AXIS2_PLACEMENT_3D('',#9865,#7852,#7853);
#6833=AXIS2_PLACEMENT_3D('',#9872,#7857,#7858);
#6834=AXIS2_PLACEMENT_3D('',#9873,#7859,#7860);
#6835=AXIS2_PLACEMENT_3D('',#9887,#7868,#7869);
#6836=AXIS2_PLACEMENT_3D('',#9891,#7872,#7873);
#6837=AXIS2_PLACEMENT_3D('',#9895,#7876,#7877);
#6838=AXIS2_PLACEMENT_3D('',#9905,#7883,#7884);
#6839=AXIS2_PLACEMENT_3D('',#9907,#7886,#7887);
#6840=AXIS2_PLACEMENT_3D('',#9911,#7889,#7890);
#6841=AXIS2_PLACEMENT_3D('',#9913,#7892,#7893);
#6842=AXIS2_PLACEMENT_3D('',#9915,#7894,#7895);
#6843=AXIS2_PLACEMENT_3D('',#9918,#7897,#7898);
#6844=AXIS2_PLACEMENT_3D('',#9920,#7899,#7900);
#6845=AXIS2_PLACEMENT_3D('',#9921,#7901,#7902);
#6846=AXIS2_PLACEMENT_3D('',#9922,#7903,#7904);
#6847=AXIS2_PLACEMENT_3D('',#9924,#7906,#7907);
#6848=AXIS2_PLACEMENT_3D('',#9926,#7909,#7910);
#6849=AXIS2_PLACEMENT_3D('',#9928,#7912,#7913);
#6850=AXIS2_PLACEMENT_3D('',#9929,#7914,#7915);
#6851=AXIS2_PLACEMENT_3D('',#9930,#7916,#7917);
#6852=AXIS2_PLACEMENT_3D('',#9932,#7918,#7919);
#6853=AXIS2_PLACEMENT_3D('',#9935,#7921,#7922);
#6854=AXIS2_PLACEMENT_3D('',#9936,#7923,#7924);
#6855=AXIS2_PLACEMENT_3D('',#9939,#7926,#7927);
#6856=AXIS2_PLACEMENT_3D('',#9940,#7928,#7929);
#6857=AXIS2_PLACEMENT_3D('',#9942,#7930,#7931);
#6858=AXIS2_PLACEMENT_3D('',#9943,#7932,#7933);
#6859=AXIS2_PLACEMENT_3D('',#9946,#7935,#7936);
#6860=AXIS2_PLACEMENT_3D('',#9947,#7937,#7938);
#6861=AXIS2_PLACEMENT_3D('',#9948,#7939,#7940);
#6862=AXIS2_PLACEMENT_3D('',#9949,#7941,#7942);
#6863=AXIS2_PLACEMENT_3D('',#9958,#7947,#7948);
#6864=AXIS2_PLACEMENT_3D('',#9964,#7952,#7953);
#6865=AXIS2_PLACEMENT_3D('',#9970,#7957,#7958);
#6866=AXIS2_PLACEMENT_3D('',#9973,#7961,#7962);
#6867=AXIS2_PLACEMENT_3D('',#9974,#7963,#7964);
#6868=AXIS2_PLACEMENT_3D('',#9975,#7965,#7966);
#6869=AXIS2_PLACEMENT_3D('',#9976,#7967,#7968);
#6870=AXIS2_PLACEMENT_3D('',#9985,#7973,#7974);
#6871=AXIS2_PLACEMENT_3D('',#9991,#7978,#7979);
#6872=AXIS2_PLACEMENT_3D('',#9997,#7983,#7984);
#6873=AXIS2_PLACEMENT_3D('',#10000,#7987,#7988);
#6874=AXIS2_PLACEMENT_3D('',#10001,#7989,#7990);
#6875=AXIS2_PLACEMENT_3D('',#10002,#7991,#7992);
#6876=AXIS2_PLACEMENT_3D('',#10003,#7993,#7994);
#6877=AXIS2_PLACEMENT_3D('',#10005,#7995,#7996);
#6878=AXIS2_PLACEMENT_3D('',#10008,#7998,#7999);
#6879=AXIS2_PLACEMENT_3D('',#10009,#8000,#8001);
#6880=AXIS2_PLACEMENT_3D('',#10011,#8002,#8003);
#6881=AXIS2_PLACEMENT_3D('',#10014,#8005,#8006);
#6882=AXIS2_PLACEMENT_3D('',#10015,#8007,#8008);
#6883=AXIS2_PLACEMENT_3D('',#10018,#8009,#8010);
#6884=AXIS2_PLACEMENT_3D('',#10022,#8012,#8013);
#6885=AXIS2_PLACEMENT_3D('',#10024,#8015,#8016);
#6886=AXIS2_PLACEMENT_3D('',#10035,#8022,#8023);
#6887=AXIS2_PLACEMENT_3D('',#10037,#8024,#8025);
#6888=AXIS2_PLACEMENT_3D('',#10038,#8026,#8027);
#6889=AXIS2_PLACEMENT_3D('',#10042,#8030,#8031);
#6890=AXIS2_PLACEMENT_3D('',#10044,#8032,#8033);
#6891=AXIS2_PLACEMENT_3D('',#10046,#8035,#8036);
#6892=AXIS2_PLACEMENT_3D('',#10048,#8037,#8038);
#6893=AXIS2_PLACEMENT_3D('',#10050,#8040,#8041);
#6894=AXIS2_PLACEMENT_3D('',#10059,#8046,#8047);
#6895=AXIS2_PLACEMENT_3D('',#10065,#8051,#8052);
#6896=AXIS2_PLACEMENT_3D('',#10068,#8055,#8056);
#6897=AXIS2_PLACEMENT_3D('',#10072,#8059,#8060);
#6898=AXIS2_PLACEMENT_3D('',#10075,#8063,#8064);
#6899=AXIS2_PLACEMENT_3D('',#10076,#8065,#8066);
#6900=AXIS2_PLACEMENT_3D('',#10077,#8067,#8068);
#6901=AXIS2_PLACEMENT_3D('',#10078,#8069,#8070);
#6902=AXIS2_PLACEMENT_3D('',#10080,#8071,#8072);
#6903=AXIS2_PLACEMENT_3D('',#10083,#8074,#8075);
#6904=AXIS2_PLACEMENT_3D('',#10084,#8076,#8077);
#6905=AXIS2_PLACEMENT_3D('',#10085,#8078,#8079);
#6906=AXIS2_PLACEMENT_3D('',#10087,#8080,#8081);
#6907=AXIS2_PLACEMENT_3D('',#10089,#8082,#8083);
#6908=AXIS2_PLACEMENT_3D('',#10090,#8084,#8085);
#6909=AXIS2_PLACEMENT_3D('',#10093,#8087,#8088);
#6910=AXIS2_PLACEMENT_3D('',#10094,#8089,#8090);
#6911=AXIS2_PLACEMENT_3D('',#10095,#8091,#8092);
#6912=AXIS2_PLACEMENT_3D('',#10097,#8093,#8094);
#6913=AXIS2_PLACEMENT_3D('',#10099,#8096,#8097);
#6914=AXIS2_PLACEMENT_3D('',#10100,#8098,#8099);
#6915=AXIS2_PLACEMENT_3D('',#10101,#8100,#8101);
#6916=AXIS2_PLACEMENT_3D('',#10103,#8102,#8103);
#6917=AXIS2_PLACEMENT_3D('',#10106,#8105,#8106);
#6918=AXIS2_PLACEMENT_3D('',#10107,#8107,#8108);
#6919=AXIS2_PLACEMENT_3D('',#10109,#8109,#8110);
#6920=AXIS2_PLACEMENT_3D('',#10112,#8112,#8113);
#6921=AXIS2_PLACEMENT_3D('',#10113,#8114,#8115);
#6922=AXIS2_PLACEMENT_3D('',#10114,#8116,#8117);
#6923=AXIS2_PLACEMENT_3D('',#10115,#8118,#8119);
#6924=AXIS2_PLACEMENT_3D('',#10116,#8120,#8121);
#6925=AXIS2_PLACEMENT_3D('',#10118,#8122,#8123);
#6926=AXIS2_PLACEMENT_3D('',#10121,#8125,#8126);
#6927=AXIS2_PLACEMENT_3D('',#10122,#8127,#8128);
#6928=AXIS2_PLACEMENT_3D('',#10124,#8129,#8130);
#6929=AXIS2_PLACEMENT_3D('',#10127,#8132,#8133);
#6930=AXIS2_PLACEMENT_3D('',#10128,#8134,#8135);
#6931=AXIS2_PLACEMENT_3D('',#10129,#8136,#8137);
#6932=AXIS2_PLACEMENT_3D('',#10130,#8138,#8139);
#6933=AXIS2_PLACEMENT_3D('',#10131,#8140,#8141);
#6934=AXIS2_PLACEMENT_3D('',#10133,#8142,#8143);
#6935=AXIS2_PLACEMENT_3D('',#10136,#8145,#8146);
#6936=AXIS2_PLACEMENT_3D('',#10137,#8147,#8148);
#6937=AXIS2_PLACEMENT_3D('',#10139,#8149,#8150);
#6938=AXIS2_PLACEMENT_3D('',#10142,#8152,#8153);
#6939=AXIS2_PLACEMENT_3D('',#10143,#8154,#8155);
#6940=AXIS2_PLACEMENT_3D('',#10144,#8156,#8157);
#6941=AXIS2_PLACEMENT_3D('',#10145,#8158,#8159);
#6942=AXIS2_PLACEMENT_3D('',#10146,#8160,#8161);
#6943=AXIS2_PLACEMENT_3D('',#10148,#8162,#8163);
#6944=AXIS2_PLACEMENT_3D('',#10151,#8165,#8166);
#6945=AXIS2_PLACEMENT_3D('',#10152,#8167,#8168);
#6946=AXIS2_PLACEMENT_3D('',#10153,#8169,#8170);
#6947=AXIS2_PLACEMENT_3D('',#10155,#8171,#8172);
#6948=AXIS2_PLACEMENT_3D('',#10157,#8173,#8174);
#6949=AXIS2_PLACEMENT_3D('',#10158,#8175,#8176);
#6950=AXIS2_PLACEMENT_3D('',#10161,#8178,#8179);
#6951=AXIS2_PLACEMENT_3D('',#10162,#8180,#8181);
#6952=AXIS2_PLACEMENT_3D('',#10163,#8182,#8183);
#6953=AXIS2_PLACEMENT_3D('',#10165,#8184,#8185);
#6954=AXIS2_PLACEMENT_3D('',#10167,#8187,#8188);
#6955=AXIS2_PLACEMENT_3D('',#10168,#8189,#8190);
#6956=AXIS2_PLACEMENT_3D('',#10169,#8191,#8192);
#6957=AXIS2_PLACEMENT_3D('',#10171,#8193,#8194);
#6958=AXIS2_PLACEMENT_3D('',#10174,#8196,#8197);
#6959=AXIS2_PLACEMENT_3D('',#10175,#8198,#8199);
#6960=AXIS2_PLACEMENT_3D('',#10177,#8200,#8201);
#6961=AXIS2_PLACEMENT_3D('',#10180,#8203,#8204);
#6962=AXIS2_PLACEMENT_3D('',#10181,#8205,#8206);
#6963=AXIS2_PLACEMENT_3D('',#10182,#8207,#8208);
#6964=AXIS2_PLACEMENT_3D('',#10183,#8209,#8210);
#6965=AXIS2_PLACEMENT_3D('',#10184,#8211,#8212);
#6966=AXIS2_PLACEMENT_3D('',#10186,#8213,#8214);
#6967=AXIS2_PLACEMENT_3D('',#10189,#8216,#8217);
#6968=AXIS2_PLACEMENT_3D('',#10190,#8218,#8219);
#6969=AXIS2_PLACEMENT_3D('',#10192,#8220,#8221);
#6970=AXIS2_PLACEMENT_3D('',#10195,#8223,#8224);
#6971=AXIS2_PLACEMENT_3D('',#10196,#8225,#8226);
#6972=AXIS2_PLACEMENT_3D('',#10197,#8227,#8228);
#6973=AXIS2_PLACEMENT_3D('',#10198,#8229,#8230);
#6974=AXIS2_PLACEMENT_3D('',#10199,#8231,#8232);
#6975=AXIS2_PLACEMENT_3D('',#10201,#8233,#8234);
#6976=AXIS2_PLACEMENT_3D('',#10204,#8236,#8237);
#6977=AXIS2_PLACEMENT_3D('',#10205,#8238,#8239);
#6978=AXIS2_PLACEMENT_3D('',#10207,#8240,#8241);
#6979=AXIS2_PLACEMENT_3D('',#10210,#8243,#8244);
#6980=AXIS2_PLACEMENT_3D('',#10211,#8245,#8246);
#6981=AXIS2_PLACEMENT_3D('',#10214,#8247,#8248);
#6982=AXIS2_PLACEMENT_3D('',#10218,#8250,#8251);
#6983=AXIS2_PLACEMENT_3D('',#10220,#8253,#8254);
#6984=AXIS2_PLACEMENT_3D('',#10231,#8260,#8261);
#6985=AXIS2_PLACEMENT_3D('',#10233,#8262,#8263);
#6986=AXIS2_PLACEMENT_3D('',#10234,#8264,#8265);
#6987=AXIS2_PLACEMENT_3D('',#10238,#8268,#8269);
#6988=AXIS2_PLACEMENT_3D('',#10240,#8270,#8271);
#6989=AXIS2_PLACEMENT_3D('',#10242,#8273,#8274);
#6990=AXIS2_PLACEMENT_3D('',#10244,#8275,#8276);
#6991=AXIS2_PLACEMENT_3D('',#10246,#8278,#8279);
#6992=AXIS2_PLACEMENT_3D('',#10255,#8284,#8285);
#6993=AXIS2_PLACEMENT_3D('',#10261,#8289,#8290);
#6994=AXIS2_PLACEMENT_3D('',#10264,#8293,#8294);
#6995=AXIS2_PLACEMENT_3D('',#10268,#8297,#8298);
#6996=AXIS2_PLACEMENT_3D('',#10271,#8301,#8302);
#6997=AXIS2_PLACEMENT_3D('',#10272,#8303,#8304);
#6998=AXIS2_PLACEMENT_3D('',#10273,#8305,#8306);
#6999=AXIS2_PLACEMENT_3D('',#10274,#8307,#8308);
#7000=AXIS2_PLACEMENT_3D('',#10283,#8313,#8314);
#7001=AXIS2_PLACEMENT_3D('',#10289,#8318,#8319);
#7002=AXIS2_PLACEMENT_3D('',#10295,#8323,#8324);
#7003=AXIS2_PLACEMENT_3D('',#10301,#8328,#8329);
#7004=AXIS2_PLACEMENT_3D('',#10307,#8333,#8334);
#7005=AXIS2_PLACEMENT_3D('',#10310,#8337,#8338);
#7006=AXIS2_PLACEMENT_3D('',#10311,#8339,#8340);
#7007=AXIS2_PLACEMENT_3D('',#10312,#8341,#8342);
#7008=AXIS2_PLACEMENT_3D('',#10314,#8343,#8344);
#7009=AXIS2_PLACEMENT_3D('',#10315,#8345,#8346);
#7010=AXIS2_PLACEMENT_3D('',#10317,#8347,#8348);
#7011=AXIS2_PLACEMENT_3D('',#10318,#8349,#8350);
#7012=AXIS2_PLACEMENT_3D('',#10320,#8351,#8352);
#7013=AXIS2_PLACEMENT_3D('',#10322,#8354,#8355);
#7014=AXIS2_PLACEMENT_3D('',#10324,#8356,#8357);
#7015=AXIS2_PLACEMENT_3D('',#10326,#8359,#8360);
#7016=AXIS2_PLACEMENT_3D('',#10328,#8361,#8362);
#7017=AXIS2_PLACEMENT_3D('',#10330,#8364,#8365);
#7018=AXIS2_PLACEMENT_3D('',#10332,#8366,#8367);
#7019=AXIS2_PLACEMENT_3D('',#10333,#8368,#8369);
#7020=AXIS2_PLACEMENT_3D('',#10335,#8370,#8371);
#7021=AXIS2_PLACEMENT_3D('',#10337,#8373,#8374);
#7022=AXIS2_PLACEMENT_3D('',#10339,#8376,#8377);
#7023=AXIS2_PLACEMENT_3D('',#10340,#8378,#8379);
#7024=AXIS2_PLACEMENT_3D('',#10342,#8380,#8381);
#7025=AXIS2_PLACEMENT_3D('',#10345,#8383,#8384);
#7026=AXIS2_PLACEMENT_3D('',#10346,#8385,#8386);
#7027=AXIS2_PLACEMENT_3D('',#10347,#8387,#8388);
#7028=AXIS2_PLACEMENT_3D('',#10349,#8389,#8390);
#7029=AXIS2_PLACEMENT_3D('',#10351,#8391,#8392);
#7030=AXIS2_PLACEMENT_3D('',#10352,#8393,#8394);
#7031=AXIS2_PLACEMENT_3D('',#10355,#8396,#8397);
#7032=AXIS2_PLACEMENT_3D('',#10356,#8398,#8399);
#7033=AXIS2_PLACEMENT_3D('',#10357,#8400,#8401);
#7034=AXIS2_PLACEMENT_3D('',#10359,#8402,#8403);
#7035=AXIS2_PLACEMENT_3D('',#10361,#8405,#8406);
#7036=AXIS2_PLACEMENT_3D('',#10362,#8407,#8408);
#7037=AXIS2_PLACEMENT_3D('',#10363,#8409,#8410);
#7038=AXIS2_PLACEMENT_3D('',#10365,#8411,#8412);
#7039=AXIS2_PLACEMENT_3D('',#10368,#8414,#8415);
#7040=AXIS2_PLACEMENT_3D('',#10369,#8416,#8417);
#7041=AXIS2_PLACEMENT_3D('',#10371,#8418,#8419);
#7042=AXIS2_PLACEMENT_3D('',#10374,#8421,#8422);
#7043=AXIS2_PLACEMENT_3D('',#10375,#8423,#8424);
#7044=AXIS2_PLACEMENT_3D('',#10376,#8425,#8426);
#7045=AXIS2_PLACEMENT_3D('',#10377,#8427,#8428);
#7046=AXIS2_PLACEMENT_3D('',#10378,#8429,#8430);
#7047=AXIS2_PLACEMENT_3D('',#10380,#8431,#8432);
#7048=AXIS2_PLACEMENT_3D('',#10383,#8434,#8435);
#7049=AXIS2_PLACEMENT_3D('',#10384,#8436,#8437);
#7050=AXIS2_PLACEMENT_3D('',#10386,#8438,#8439);
#7051=AXIS2_PLACEMENT_3D('',#10389,#8441,#8442);
#7052=AXIS2_PLACEMENT_3D('',#10390,#8443,#8444);
#7053=AXIS2_PLACEMENT_3D('',#10391,#8445,#8446);
#7054=AXIS2_PLACEMENT_3D('',#10392,#8447,#8448);
#7055=AXIS2_PLACEMENT_3D('',#10393,#8449,#8450);
#7056=AXIS2_PLACEMENT_3D('',#10395,#8451,#8452);
#7057=AXIS2_PLACEMENT_3D('',#10398,#8454,#8455);
#7058=AXIS2_PLACEMENT_3D('',#10399,#8456,#8457);
#7059=AXIS2_PLACEMENT_3D('',#10400,#8458,#8459);
#7060=AXIS2_PLACEMENT_3D('',#10402,#8460,#8461);
#7061=AXIS2_PLACEMENT_3D('',#10404,#8462,#8463);
#7062=AXIS2_PLACEMENT_3D('',#10405,#8464,#8465);
#7063=AXIS2_PLACEMENT_3D('',#10408,#8467,#8468);
#7064=AXIS2_PLACEMENT_3D('',#10409,#8469,#8470);
#7065=AXIS2_PLACEMENT_3D('',#10410,#8471,#8472);
#7066=AXIS2_PLACEMENT_3D('',#10412,#8473,#8474);
#7067=AXIS2_PLACEMENT_3D('',#10414,#8476,#8477);
#7068=AXIS2_PLACEMENT_3D('',#10415,#8478,#8479);
#7069=AXIS2_PLACEMENT_3D('',#10416,#8480,#8481);
#7070=AXIS2_PLACEMENT_3D('',#10418,#8482,#8483);
#7071=AXIS2_PLACEMENT_3D('',#10421,#8485,#8486);
#7072=AXIS2_PLACEMENT_3D('',#10422,#8487,#8488);
#7073=AXIS2_PLACEMENT_3D('',#10424,#8489,#8490);
#7074=AXIS2_PLACEMENT_3D('',#10427,#8492,#8493);
#7075=AXIS2_PLACEMENT_3D('',#10428,#8494,#8495);
#7076=AXIS2_PLACEMENT_3D('',#10429,#8496,#8497);
#7077=AXIS2_PLACEMENT_3D('',#10430,#8498,#8499);
#7078=AXIS2_PLACEMENT_3D('',#10431,#8500,#8501);
#7079=AXIS2_PLACEMENT_3D('',#10433,#8502,#8503);
#7080=AXIS2_PLACEMENT_3D('',#10436,#8505,#8506);
#7081=AXIS2_PLACEMENT_3D('',#10437,#8507,#8508);
#7082=AXIS2_PLACEMENT_3D('',#10439,#8509,#8510);
#7083=AXIS2_PLACEMENT_3D('',#10442,#8512,#8513);
#7084=AXIS2_PLACEMENT_3D('',#10443,#8514,#8515);
#7085=AXIS2_PLACEMENT_3D('',#10444,#8516,#8517);
#7086=AXIS2_PLACEMENT_3D('',#10445,#8518,#8519);
#7087=AXIS2_PLACEMENT_3D('',#10446,#8520,#8521);
#7088=AXIS2_PLACEMENT_3D('',#10455,#8526,#8527);
#7089=AXIS2_PLACEMENT_3D('',#10461,#8531,#8532);
#7090=AXIS2_PLACEMENT_3D('',#10467,#8536,#8537);
#7091=AXIS2_PLACEMENT_3D('',#10473,#8541,#8542);
#7092=AXIS2_PLACEMENT_3D('',#10479,#8546,#8547);
#7093=AXIS2_PLACEMENT_3D('',#10482,#8550,#8551);
#7094=AXIS2_PLACEMENT_3D('',#10483,#8552,#8553);
#7095=AXIS2_PLACEMENT_3D('',#10484,#8554,#8555);
#7096=AXIS2_PLACEMENT_3D('',#10486,#8556,#8557);
#7097=AXIS2_PLACEMENT_3D('',#10487,#8558,#8559);
#7098=AXIS2_PLACEMENT_3D('',#10489,#8560,#8561);
#7099=AXIS2_PLACEMENT_3D('',#10490,#8562,#8563);
#7100=AXIS2_PLACEMENT_3D('',#10492,#8564,#8565);
#7101=AXIS2_PLACEMENT_3D('',#10494,#8567,#8568);
#7102=AXIS2_PLACEMENT_3D('',#10496,#8569,#8570);
#7103=AXIS2_PLACEMENT_3D('',#10498,#8572,#8573);
#7104=AXIS2_PLACEMENT_3D('',#10500,#8574,#8575);
#7105=AXIS2_PLACEMENT_3D('',#10502,#8577,#8578);
#7106=AXIS2_PLACEMENT_3D('',#10504,#8579,#8580);
#7107=AXIS2_PLACEMENT_3D('',#10505,#8581,#8582);
#7108=AXIS2_PLACEMENT_3D('',#10507,#8583,#8584);
#7109=AXIS2_PLACEMENT_3D('',#10509,#8586,#8587);
#7110=AXIS2_PLACEMENT_3D('',#10511,#8589,#8590);
#7111=AXIS2_PLACEMENT_3D('',#10512,#8591,#8592);
#7112=AXIS2_PLACEMENT_3D('',#10514,#8593,#8594);
#7113=AXIS2_PLACEMENT_3D('',#10517,#8596,#8597);
#7114=AXIS2_PLACEMENT_3D('',#10518,#8598,#8599);
#7115=AXIS2_PLACEMENT_3D('',#10519,#8600,#8601);
#7116=AXIS2_PLACEMENT_3D('',#10521,#8602,#8603);
#7117=AXIS2_PLACEMENT_3D('',#10524,#8605,#8606);
#7118=AXIS2_PLACEMENT_3D('',#10525,#8607,#8608);
#7119=AXIS2_PLACEMENT_3D('',#10527,#8609,#8610);
#7120=AXIS2_PLACEMENT_3D('',#10530,#8612,#8613);
#7121=AXIS2_PLACEMENT_3D('',#10531,#8614,#8615);
#7122=AXIS2_PLACEMENT_3D('',#10540,#8620,#8621);
#7123=AXIS2_PLACEMENT_3D('',#10546,#8625,#8626);
#7124=AXIS2_PLACEMENT_3D('',#10552,#8630,#8631);
#7125=AXIS2_PLACEMENT_3D('',#10555,#8634,#8635);
#7126=AXIS2_PLACEMENT_3D('',#10556,#8636,#8637);
#7127=AXIS2_PLACEMENT_3D('',#10557,#8638,#8639);
#7128=AXIS2_PLACEMENT_3D('',#10558,#8640,#8641);
#7129=AXIS2_PLACEMENT_3D('',#10567,#8646,#8647);
#7130=AXIS2_PLACEMENT_3D('',#10573,#8651,#8652);
#7131=AXIS2_PLACEMENT_3D('',#10579,#8656,#8657);
#7132=AXIS2_PLACEMENT_3D('',#10585,#8661,#8662);
#7133=AXIS2_PLACEMENT_3D('',#10591,#8666,#8667);
#7134=AXIS2_PLACEMENT_3D('',#10594,#8670,#8671);
#7135=AXIS2_PLACEMENT_3D('',#10595,#8672,#8673);
#7136=AXIS2_PLACEMENT_3D('',#10596,#8674,#8675);
#7137=AXIS2_PLACEMENT_3D('',#10598,#8676,#8677);
#7138=AXIS2_PLACEMENT_3D('',#10599,#8678,#8679);
#7139=AXIS2_PLACEMENT_3D('',#10601,#8680,#8681);
#7140=AXIS2_PLACEMENT_3D('',#10602,#8682,#8683);
#7141=AXIS2_PLACEMENT_3D('',#10604,#8684,#8685);
#7142=AXIS2_PLACEMENT_3D('',#10606,#8687,#8688);
#7143=AXIS2_PLACEMENT_3D('',#10608,#8689,#8690);
#7144=AXIS2_PLACEMENT_3D('',#10610,#8692,#8693);
#7145=AXIS2_PLACEMENT_3D('',#10612,#8694,#8695);
#7146=AXIS2_PLACEMENT_3D('',#10614,#8697,#8698);
#7147=AXIS2_PLACEMENT_3D('',#10616,#8699,#8700);
#7148=AXIS2_PLACEMENT_3D('',#10617,#8701,#8702);
#7149=AXIS2_PLACEMENT_3D('',#10619,#8703,#8704);
#7150=AXIS2_PLACEMENT_3D('',#10621,#8706,#8707);
#7151=AXIS2_PLACEMENT_3D('',#10623,#8709,#8710);
#7152=AXIS2_PLACEMENT_3D('',#10624,#8711,#8712);
#7153=AXIS2_PLACEMENT_3D('',#10629,#8714,#8715);
#7154=AXIS2_PLACEMENT_3D('',#10630,#8716,#8717);
#7155=AXIS2_PLACEMENT_3D('',#10631,#8718,#8719);
#7156=AXIS2_PLACEMENT_3D('',#10644,#8720,#8721);
#7157=AXIS2_PLACEMENT_3D('',#10657,#8723,#8724);
#7158=AXIS2_PLACEMENT_3D('',#10658,#8725,#8726);
#7159=AXIS2_PLACEMENT_3D('',#10660,#8728,#8729);
#7160=AXIS2_PLACEMENT_3D('',#10665,#8731,#8732);
#7161=AXIS2_PLACEMENT_3D('',#10666,#8733,#8734);
#7162=AXIS2_PLACEMENT_3D('',#10667,#8735,#8736);
#7163=AXIS2_PLACEMENT_3D('',#10684,#8737,#8738);
#7164=AXIS2_PLACEMENT_3D('',#10701,#8740,#8741);
#7165=AXIS2_PLACEMENT_3D('',#10702,#8742,#8743);
#7166=AXIS2_PLACEMENT_3D('',#10704,#8745,#8746);
#7167=AXIS2_PLACEMENT_3D('',#10706,#8747,#8748);
#7168=AXIS2_PLACEMENT_3D('',#10709,#8750,#8751);
#7169=AXIS2_PLACEMENT_3D('',#10710,#8752,#8753);
#7170=AXIS2_PLACEMENT_3D('',#10712,#8754,#8755);
#7171=AXIS2_PLACEMENT_3D('',#10715,#8757,#8758);
#7172=AXIS2_PLACEMENT_3D('',#10716,#8759,#8760);
#7173=AXIS2_PLACEMENT_3D('',#10725,#8765,#8766);
#7174=AXIS2_PLACEMENT_3D('',#10731,#8770,#8771);
#7175=AXIS2_PLACEMENT_3D('',#10737,#8775,#8776);
#7176=AXIS2_PLACEMENT_3D('',#10740,#8779,#8780);
#7177=AXIS2_PLACEMENT_3D('',#10741,#8781,#8782);
#7178=AXIS2_PLACEMENT_3D('',#10742,#8783,#8784);
#7179=AXIS2_PLACEMENT_3D('',#10743,#8785,#8786);
#7180=AXIS2_PLACEMENT_3D('',#10752,#8791,#8792);
#7181=AXIS2_PLACEMENT_3D('',#10758,#8796,#8797);
#7182=AXIS2_PLACEMENT_3D('',#10764,#8801,#8802);
#7183=AXIS2_PLACEMENT_3D('',#10770,#8806,#8807);
#7184=AXIS2_PLACEMENT_3D('',#10776,#8811,#8812);
#7185=AXIS2_PLACEMENT_3D('',#10779,#8815,#8816);
#7186=AXIS2_PLACEMENT_3D('',#10780,#8817,#8818);
#7187=AXIS2_PLACEMENT_3D('',#10782,#8819,#8820);
#7188=AXIS2_PLACEMENT_3D('',#10783,#8821,#8822);
#7189=AXIS2_PLACEMENT_3D('',#10785,#8823,#8824);
#7190=AXIS2_PLACEMENT_3D('',#10787,#8826,#8827);
#7191=AXIS2_PLACEMENT_3D('',#10789,#8828,#8829);
#7192=AXIS2_PLACEMENT_3D('',#10791,#8831,#8832);
#7193=AXIS2_PLACEMENT_3D('',#10793,#8833,#8834);
#7194=AXIS2_PLACEMENT_3D('',#10795,#8836,#8837);
#7195=AXIS2_PLACEMENT_3D('',#10796,#8838,#8839);
#7196=AXIS2_PLACEMENT_3D('',#10797,#8840,#8841);
#7197=AXIS2_PLACEMENT_3D('',#10799,#8842,#8843);
#7198=AXIS2_PLACEMENT_3D('',#10802,#8845,#8846);
#7199=AXIS2_PLACEMENT_3D('',#10803,#8847,#8848);
#7200=AXIS2_PLACEMENT_3D('',#10804,#8849,#8850);
#7201=AXIS2_PLACEMENT_3D('',#10845,#8852,#8853);
#7202=AXIS2_PLACEMENT_3D('',#10846,#8854,#8855);
#7203=AXIS2_PLACEMENT_3D('',#10847,#8856,#8857);
#7204=AXIS2_PLACEMENT_3D('',#10849,#8858,#8859);
#7205=AXIS2_PLACEMENT_3D('',#10852,#8861,#8862);
#7206=AXIS2_PLACEMENT_3D('',#10853,#8863,#8864);
#7207=AXIS2_PLACEMENT_3D('',#10854,#8865,#8866);
#7208=AXIS2_PLACEMENT_3D('',#10855,#8867,#8868);
#7209=AXIS2_PLACEMENT_3D('',#10856,#8869,#8870);
#7210=AXIS2_PLACEMENT_3D('',#10858,#8871,#8872);
#7211=AXIS2_PLACEMENT_3D('',#10861,#8874,#8875);
#7212=AXIS2_PLACEMENT_3D('',#10862,#8876,#8877);
#7213=AXIS2_PLACEMENT_3D('',#10863,#8878,#8879);
#7214=AXIS2_PLACEMENT_3D('',#10864,#8880,#8881);
#7215=AXIS2_PLACEMENT_3D('',#10865,#8882,#8883);
#7216=AXIS2_PLACEMENT_3D('',#10874,#8888,#8889);
#7217=AXIS2_PLACEMENT_3D('',#10880,#8893,#8894);
#7218=AXIS2_PLACEMENT_3D('',#10883,#8897,#8898);
#7219=AXIS2_PLACEMENT_3D('',#10884,#8899,#8900);
#7220=AXIS2_PLACEMENT_3D('',#10885,#8901,#8902);
#7221=AXIS2_PLACEMENT_3D('',#10886,#8903,#8904);
#7222=AXIS2_PLACEMENT_3D('',#10888,#8905,#8906);
#7223=AXIS2_PLACEMENT_3D('',#10891,#8908,#8909);
#7224=AXIS2_PLACEMENT_3D('',#10892,#8910,#8911);
#7225=AXIS2_PLACEMENT_3D('',#10893,#8912,#8913);
#7226=AXIS2_PLACEMENT_3D('',#10894,#8914,#8915);
#7227=AXIS2_PLACEMENT_3D('',#10895,#8916,#8917);
#7228=AXIS2_PLACEMENT_3D('',#10897,#8918,#8919);
#7229=AXIS2_PLACEMENT_3D('',#10900,#8921,#8922);
#7230=AXIS2_PLACEMENT_3D('',#10901,#8923,#8924);
#7231=AXIS2_PLACEMENT_3D('',#10903,#8925,#8926);
#7232=AXIS2_PLACEMENT_3D('',#10906,#8928,#8929);
#7233=AXIS2_PLACEMENT_3D('',#10907,#8930,#8931);
#7234=AXIS2_PLACEMENT_3D('',#10908,#8932,#8933);
#7235=AXIS2_PLACEMENT_3D('',#10909,#8934,#8935);
#7236=AXIS2_PLACEMENT_3D('',#10910,#8936,#8937);
#7237=AXIS2_PLACEMENT_3D('',#10912,#8938,#8939);
#7238=AXIS2_PLACEMENT_3D('',#10915,#8941,#8942);
#7239=AXIS2_PLACEMENT_3D('',#10916,#8943,#8944);
#7240=AXIS2_PLACEMENT_3D('',#10918,#8945,#8946);
#7241=AXIS2_PLACEMENT_3D('',#10921,#8948,#8949);
#7242=AXIS2_PLACEMENT_3D('',#10922,#8950,#8951);
#7243=AXIS2_PLACEMENT_3D('',#10923,#8952,#8953);
#7244=AXIS2_PLACEMENT_3D('',#10924,#8954,#8955);
#7245=AXIS2_PLACEMENT_3D('',#10925,#8956,#8957);
#7246=AXIS2_PLACEMENT_3D('',#10927,#8958,#8959);
#7247=AXIS2_PLACEMENT_3D('',#10930,#8961,#8962);
#7248=AXIS2_PLACEMENT_3D('',#10931,#8963,#8964);
#7249=AXIS2_PLACEMENT_3D('',#10933,#8965,#8966);
#7250=AXIS2_PLACEMENT_3D('',#10936,#8968,#8969);
#7251=AXIS2_PLACEMENT_3D('',#10937,#8970,#8971);
#7252=AXIS2_PLACEMENT_3D('',#10938,#8972,#8973);
#7253=AXIS2_PLACEMENT_3D('',#10939,#8974,#8975);
#7254=AXIS2_PLACEMENT_3D('',#10940,#8976,#8977);
#7255=AXIS2_PLACEMENT_3D('',#10941,#8978,#8979);
#7256=AXIS2_PLACEMENT_3D('',#10942,#8980,#8981);
#7257=AXIS2_PLACEMENT_3D('',#10943,#8982,#8983);
#7258=AXIS2_PLACEMENT_3D('',#10944,#8984,#8985);
#7259=AXIS2_PLACEMENT_3D('',#10945,#8986,#8987);
#7260=AXIS2_PLACEMENT_3D('',#10946,#8988,#8989);
#7261=AXIS2_PLACEMENT_3D('',#10947,#8990,#8991);
#7262=AXIS2_PLACEMENT_3D('',#10948,#8992,#8993);
#7263=AXIS2_PLACEMENT_3D('',#10949,#8994,#8995);
#7264=AXIS2_PLACEMENT_3D('',#10950,#8996,#8997);
#7265=AXIS2_PLACEMENT_3D('',#10951,#8998,#8999);
#7266=AXIS2_PLACEMENT_3D('',#10952,#9000,#9001);
#7267=AXIS2_PLACEMENT_3D('',#10953,#9002,#9003);
#7268=AXIS2_PLACEMENT_3D('',#10954,#9004,#9005);
#7269=AXIS2_PLACEMENT_3D('',#10955,#9006,#9007);
#7270=AXIS2_PLACEMENT_3D('',#10956,#9008,#9009);
#7271=AXIS2_PLACEMENT_3D('',#10957,#9010,#9011);
#7272=AXIS2_PLACEMENT_3D('',#10958,#9012,#9013);
#7273=AXIS2_PLACEMENT_3D('',#10959,#9014,#9015);
#7274=AXIS2_PLACEMENT_3D('',#10960,#9016,#9017);
#7275=AXIS2_PLACEMENT_3D('',#10961,#9018,#9019);
#7276=AXIS2_PLACEMENT_3D('',#10962,#9020,#9021);
#7277=AXIS2_PLACEMENT_3D('',#10963,#9022,#9023);
#7278=AXIS2_PLACEMENT_3D('',#10964,#9024,#9025);
#7279=AXIS2_PLACEMENT_3D('',#10965,#9026,#9027);
#7280=AXIS2_PLACEMENT_3D('',#10966,#9028,#9029);
#7281=AXIS2_PLACEMENT_3D('',#10967,#9030,#9031);
#7282=AXIS2_PLACEMENT_3D('',#10968,#9032,#9033);
#7283=AXIS2_PLACEMENT_3D('',#10969,#9034,#9035);
#7284=AXIS2_PLACEMENT_3D('',#10970,#9036,#9037);
#7285=AXIS2_PLACEMENT_3D('',#10971,#9038,#9039);
#7286=AXIS2_PLACEMENT_3D('',#10972,#9040,#9041);
#7287=AXIS2_PLACEMENT_3D('',#10973,#9042,#9043);
#7288=AXIS2_PLACEMENT_3D('',#10974,#9044,#9045);
#7289=AXIS2_PLACEMENT_3D('',#10975,#9046,#9047);
#7290=AXIS2_PLACEMENT_3D('',#10976,#9048,#9049);
#7291=AXIS2_PLACEMENT_3D('',#10977,#9050,#9051);
#7292=AXIS2_PLACEMENT_3D('',#10978,#9052,#9053);
#7293=AXIS2_PLACEMENT_3D('',#10979,#9054,#9055);
#7294=AXIS2_PLACEMENT_3D('',#10980,#9056,#9057);
#7295=AXIS2_PLACEMENT_3D('',#10981,#9058,#9059);
#7296=AXIS2_PLACEMENT_3D('',#10982,#9060,#9061);
#7297=AXIS2_PLACEMENT_3D('',#10983,#9062,#9063);
#7298=AXIS2_PLACEMENT_3D('',#10984,#9064,#9065);
#7299=AXIS2_PLACEMENT_3D('',#10985,#9066,#9067);
#7300=AXIS2_PLACEMENT_3D('',#10986,#9068,#9069);
#7301=AXIS2_PLACEMENT_3D('',#10987,#9070,#9071);
#7302=AXIS2_PLACEMENT_3D('',#10988,#9072,#9073);
#7303=AXIS2_PLACEMENT_3D('',#10989,#9074,#9075);
#7304=AXIS2_PLACEMENT_3D('',#10990,#9076,#9077);
#7305=AXIS2_PLACEMENT_3D('',#10991,#9078,#9079);
#7306=AXIS2_PLACEMENT_3D('',#10992,#9080,#9081);
#7307=AXIS2_PLACEMENT_3D('',#10993,#9082,#9083);
#7308=AXIS2_PLACEMENT_3D('',#10994,#9084,#9085);
#7309=AXIS2_PLACEMENT_3D('',#10995,#9086,#9087);
#7310=AXIS2_PLACEMENT_3D('',#10996,#9088,#9089);
#7311=AXIS2_PLACEMENT_3D('',#10997,#9090,#9091);
#7312=AXIS2_PLACEMENT_3D('',#10998,#9092,#9093);
#7313=AXIS2_PLACEMENT_3D('',#10999,#9094,#9095);
#7314=AXIS2_PLACEMENT_3D('',#11000,#9096,#9097);
#7315=AXIS2_PLACEMENT_3D('',#11002,#9098,#9099);
#7316=AXIS2_PLACEMENT_3D('',#11005,#9101,#9102);
#7317=AXIS2_PLACEMENT_3D('',#11006,#9103,#9104);
#7318=AXIS2_PLACEMENT_3D('',#11007,#9105,#9106);
#7319=AXIS2_PLACEMENT_3D('',#11008,#9107,#9108);
#7320=AXIS2_PLACEMENT_3D('',#11009,#9109,#9110);
#7321=AXIS2_PLACEMENT_3D('',#11010,#9111,#9112);
#7322=AXIS2_PLACEMENT_3D('',#11011,#9113,#9114);
#7323=AXIS2_PLACEMENT_3D('',#11012,#9115,#9116);
#7324=AXIS2_PLACEMENT_3D('',#11015,#9117,#9118);
#7325=AXIS2_PLACEMENT_3D('',#11016,#9119,#9120);
#7326=AXIS2_PLACEMENT_3D('',#11018,#9121,#9122);
#7327=AXIS2_PLACEMENT_3D('',#11020,#9123,#9124);
#7328=AXIS2_PLACEMENT_3D('',#11021,#9125,#9126);
#7329=AXIS2_PLACEMENT_3D('',#11022,#9127,#9128);
#7330=AXIS2_PLACEMENT_3D('',#11025,#9130,#9131);
#7331=AXIS2_PLACEMENT_3D('',#11026,#9132,#9133);
#7332=AXIS2_PLACEMENT_3D('',#11028,#9134,#9135);
#7333=AXIS2_PLACEMENT_3D('',#11031,#9137,#9138);
#7334=AXIS2_PLACEMENT_3D('',#11032,#9139,#9140);
#7335=AXIS2_PLACEMENT_3D('',#11035,#9142,#9143);
#7336=AXIS2_PLACEMENT_3D('',#11036,#9144,#9145);
#7337=AXIS2_PLACEMENT_3D('',#11037,#9146,#9147);
#7338=AXIS2_PLACEMENT_3D('',#11039,#9148,#9149);
#7339=AXIS2_PLACEMENT_3D('',#11041,#9151,#9152);
#7340=AXIS2_PLACEMENT_3D('',#11043,#9153,#9154);
#7341=AXIS2_PLACEMENT_3D('',#11044,#9155,#9156);
#7342=AXIS2_PLACEMENT_3D('',#11046,#9158,#9159);
#7343=AXIS2_PLACEMENT_3D('',#11047,#9160,#9161);
#7344=AXIS2_PLACEMENT_3D('',#11050,#9162,#9163);
#7345=AXIS2_PLACEMENT_3D('',#11051,#9164,#9165);
#7346=AXIS2_PLACEMENT_3D('',#11053,#9166,#9167);
#7347=AXIS2_PLACEMENT_3D('',#11055,#9168,#9169);
#7348=AXIS2_PLACEMENT_3D('',#11056,#9170,#9171);
#7349=AXIS2_PLACEMENT_3D('',#11057,#9172,#9173);
#7350=AXIS2_PLACEMENT_3D('',#11059,#9174,#9175);
#7351=AXIS2_PLACEMENT_3D('',#11061,#9177,#9178);
#7352=AXIS2_PLACEMENT_3D('',#11063,#9179,#9180);
#7353=AXIS2_PLACEMENT_3D('',#11065,#9181,#9182);
#7354=AXIS2_PLACEMENT_3D('',#11066,#9183,#9184);
#7355=AXIS2_PLACEMENT_3D('',#11068,#9185,#9186);
#7356=AXIS2_PLACEMENT_3D('',#11070,#9188,#9189);
#7357=AXIS2_PLACEMENT_3D('',#11072,#9190,#9191);
#7358=AXIS2_PLACEMENT_3D('',#11074,#9193,#9194);
#7359=AXIS2_PLACEMENT_3D('',#11076,#9195,#9196);
#7360=AXIS2_PLACEMENT_3D('',#11078,#9198,#9199);
#7361=AXIS2_PLACEMENT_3D('',#11079,#9200,#9201);
#7362=AXIS2_PLACEMENT_3D('',#11081,#9203,#9204);
#7363=AXIS2_PLACEMENT_3D('',#11082,#9205,#9206);
#7364=AXIS2_PLACEMENT_3D('',#11085,#9207,#9208);
#7365=AXIS2_PLACEMENT_3D('',#11086,#9209,#9210);
#7366=AXIS2_PLACEMENT_3D('',#11089,#9211,#9212);
#7367=AXIS2_PLACEMENT_3D('',#11090,#9213,#9214);
#7368=AXIS2_PLACEMENT_3D('',#11093,#9215,#9216);
#7369=AXIS2_PLACEMENT_3D('',#11094,#9217,#9218);
#7370=AXIS2_PLACEMENT_3D('',#11097,#9219,#9220);
#7371=AXIS2_PLACEMENT_3D('',#11098,#9221,#9222);
#7372=AXIS2_PLACEMENT_3D('',#11101,#9223,#9224);
#7373=AXIS2_PLACEMENT_3D('',#11102,#9225,#9226);
#7374=AXIS2_PLACEMENT_3D('',#11105,#9227,#9228);
#7375=AXIS2_PLACEMENT_3D('',#11106,#9229,#9230);
#7376=AXIS2_PLACEMENT_3D('',#11109,#9231,#9232);
#7377=AXIS2_PLACEMENT_3D('',#11110,#9233,#9234);
#7378=AXIS2_PLACEMENT_3D('',#11113,#9235,#9236);
#7379=AXIS2_PLACEMENT_3D('',#11114,#9237,#9238);
#7380=AXIS2_PLACEMENT_3D('',#11115,#9239,#9240);
#7381=AXIS2_PLACEMENT_3D('',#11141,#9241,#9242);
#7382=AXIS2_PLACEMENT_3D('',#11165,#9243,#9244);
#7383=AXIS2_PLACEMENT_3D('',#11166,#9245,#9246);
#7384=AXIS2_PLACEMENT_3D('',#11168,#9247,#9248);
#7385=AXIS2_PLACEMENT_3D('',#11193,#9249,#9250);
#7386=AXIS2_PLACEMENT_3D('',#11218,#9251,#9252);
#7387=AXIS2_PLACEMENT_3D('',#11234,#9254,#9255);
#7388=AXIS2_PLACEMENT_3D('',#11249,#9256,#9257);
#7389=AXIS2_PLACEMENT_3D('',#11274,#9258,#9259);
#7390=AXIS2_PLACEMENT_3D('',#11299,#9260,#9261);
#7391=AXIS2_PLACEMENT_3D('',#11324,#9262,#9263);
#7392=AXIS2_PLACEMENT_3D('',#11348,#9264,#9265);
#7393=AXIS2_PLACEMENT_3D('',#11349,#9266,#9267);
#7394=AXIS2_PLACEMENT_3D('',#11351,#9268,#9269);
#7395=AXIS2_PLACEMENT_3D('',#11352,#9270,#9271);
#7396=AXIS2_PLACEMENT_3D('',#11353,#9272,#9273);
#7397=AXIS2_PLACEMENT_3D('',#11377,#9274,#9275);
#7398=AXIS2_PLACEMENT_3D('',#11378,#9276,#9277);
#7399=AXIS2_PLACEMENT_3D('',#11380,#9278,#9279);
#7400=AXIS2_PLACEMENT_3D('',#11381,#9280,#9281);
#7401=AXIS2_PLACEMENT_3D('',#11382,#9282,#9283);
#7402=AXIS2_PLACEMENT_3D('',#11406,#9284,#9285);
#7403=AXIS2_PLACEMENT_3D('',#11407,#9286,#9287);
#7404=AXIS2_PLACEMENT_3D('',#11409,#9288,#9289);
#7405=AXIS2_PLACEMENT_3D('',#11410,#9290,#9291);
#7406=AXIS2_PLACEMENT_3D('',#11411,#9292,#9293);
#7407=AXIS2_PLACEMENT_3D('',#11426,#9294,#9295);
#7408=AXIS2_PLACEMENT_3D('',#11439,#9296,#9297);
#7409=AXIS2_PLACEMENT_3D('',#11441,#9298,#9299);
#7410=AXIS2_PLACEMENT_3D('',#11442,#9300,#9301);
#7411=AXIS2_PLACEMENT_3D('',#11443,#9302,#9303);
#7412=AXIS2_PLACEMENT_3D('',#11467,#9304,#9305);
#7413=AXIS2_PLACEMENT_3D('',#11468,#9306,#9307);
#7414=AXIS2_PLACEMENT_3D('',#11470,#9308,#9309);
#7415=AXIS2_PLACEMENT_3D('',#11471,#9310,#9311);
#7416=AXIS2_PLACEMENT_3D('',#11472,#9312,#9313);
#7417=AXIS2_PLACEMENT_3D('',#11496,#9314,#9315);
#7418=AXIS2_PLACEMENT_3D('',#11497,#9316,#9317);
#7419=AXIS2_PLACEMENT_3D('',#11499,#9318,#9319);
#7420=AXIS2_PLACEMENT_3D('',#11500,#9320,#9321);
#7421=AXIS2_PLACEMENT_3D('',#11501,#9322,#9323);
#7422=AXIS2_PLACEMENT_3D('',#11525,#9324,#9325);
#7423=AXIS2_PLACEMENT_3D('',#11526,#9326,#9327);
#7424=AXIS2_PLACEMENT_3D('',#11528,#9328,#9329);
#7425=AXIS2_PLACEMENT_3D('',#11531,#9331,#9332);
#7426=AXIS2_PLACEMENT_3D('',#11555,#9333,#9334);
#7427=AXIS2_PLACEMENT_3D('',#11556,#9335,#9336);
#7428=AXIS2_PLACEMENT_3D('',#11557,#9337,#9338);
#7429=AXIS2_PLACEMENT_3D('',#11558,#9339,#9340);
#7430=AXIS2_PLACEMENT_3D('',#11559,#9341,#9342);
#7431=AXIS2_PLACEMENT_3D('',#11560,#9343,#9344);
#7432=AXIS2_PLACEMENT_3D('',#11561,#9345,#9346);
#7433=AXIS2_PLACEMENT_3D('',#11562,#9347,#9348);
#7434=AXIS2_PLACEMENT_3D('',#11563,#9349,#9350);
#7435=AXIS2_PLACEMENT_3D('',#11565,#9351,#9352);
#7436=AXIS2_PLACEMENT_3D('',#11567,#9353,#9354);
#7437=AXIS2_PLACEMENT_3D('',#11568,#9355,#9356);
#7438=AXIS2_PLACEMENT_3D('',#11570,#9357,#9358);
#7439=AXIS2_PLACEMENT_3D('',#11572,#9360,#9361);
#7440=AXIS2_PLACEMENT_3D('',#11574,#9362,#9363);
#7441=AXIS2_PLACEMENT_3D('',#11575,#9364,#9365);
#7442=AXIS2_PLACEMENT_3D('',#11577,#9367,#9368);
#7443=AXIS2_PLACEMENT_3D('',#11579,#9369,#9370);
#7444=AXIS2_PLACEMENT_3D('',#11581,#9371,#9372);
#7445=AXIS2_PLACEMENT_3D('',#11582,#9373,#9374);
#7446=AXIS2_PLACEMENT_3D('',#11584,#9375,#9376);
#7447=AXIS2_PLACEMENT_3D('',#11586,#9378,#9379);
#7448=AXIS2_PLACEMENT_3D('',#11588,#9380,#9381);
#7449=AXIS2_PLACEMENT_3D('',#11589,#9382,#9383);
#7450=AXIS2_PLACEMENT_3D('',#11591,#9385,#9386);
#7451=AXIS2_PLACEMENT_3D('',#11592,#9387,#9388);
#7452=AXIS2_PLACEMENT_3D('',#11593,#9389,#9390);
#7453=AXIS2_PLACEMENT_3D('',#11594,#9391,#9392);
#7454=AXIS2_PLACEMENT_3D('',#11595,#9393,#9394);
#7455=AXIS2_PLACEMENT_3D('',#11596,#9395,#9396);
#7456=AXIS2_PLACEMENT_3D('',#11597,#9397,#9398);
#7457=AXIS2_PLACEMENT_3D('',#11599,#9399,#9400);
#7458=AXIS2_PLACEMENT_3D('',#11602,#9402,#9403);
#7459=AXIS2_PLACEMENT_3D('',#11603,#9404,#9405);
#7460=AXIS2_PLACEMENT_3D('',#11605,#9406,#9407);
#7461=AXIS2_PLACEMENT_3D('',#11608,#9409,#9410);
#7462=AXIS2_PLACEMENT_3D('',#11609,#9411,#9412);
#7463=AXIS2_PLACEMENT_3D('',#11610,#9413,#9414);
#7464=AXIS2_PLACEMENT_3D('',#11611,#9415,#9416);
#7465=AXIS2_PLACEMENT_3D('',#11612,#9417,#9418);
#7466=AXIS2_PLACEMENT_3D('',#11614,#9419,#9420);
#7467=AXIS2_PLACEMENT_3D('',#11617,#9422,#9423);
#7468=AXIS2_PLACEMENT_3D('',#11618,#9424,#9425);
#7469=AXIS2_PLACEMENT_3D('',#11620,#9426,#9427);
#7470=AXIS2_PLACEMENT_3D('',#11623,#9429,#9430);
#7471=AXIS2_PLACEMENT_3D('',#11624,#9431,#9432);
#7472=AXIS2_PLACEMENT_3D('',#11625,#9433,#9434);
#7473=AXIS2_PLACEMENT_3D('',#11626,#9435,#9436);
#7474=AXIS2_PLACEMENT_3D('',#11627,#9437,#9438);
#7475=AXIS2_PLACEMENT_3D('',#11629,#9439,#9440);
#7476=AXIS2_PLACEMENT_3D('',#11632,#9442,#9443);
#7477=AXIS2_PLACEMENT_3D('',#11633,#9444,#9445);
#7478=AXIS2_PLACEMENT_3D('',#11635,#9446,#9447);
#7479=AXIS2_PLACEMENT_3D('',#11638,#9449,#9450);
#7480=AXIS2_PLACEMENT_3D('',#11639,#9451,#9452);
#7481=AXIS2_PLACEMENT_3D('',#11640,#9453,#9454);
#7482=AXIS2_PLACEMENT_3D('',#11641,#9455,#9456);
#7483=AXIS2_PLACEMENT_3D('',#11642,#9457,#9458);
#7484=AXIS2_PLACEMENT_3D('',#11643,#9459,#9460);
#7485=AXIS2_PLACEMENT_3D('',#11644,#9461,#9462);
#7486=AXIS2_PLACEMENT_3D('',#11645,#9463,#9464);
#7487=AXIS2_PLACEMENT_3D('',#11646,#9465,#9466);
#7488=AXIS2_PLACEMENT_3D('',#11647,#9467,#9468);
#7489=AXIS2_PLACEMENT_3D('',#11648,#9469,#9470);
#7490=AXIS2_PLACEMENT_3D('',#11649,#9471,#9472);
#7491=AXIS2_PLACEMENT_3D('',#11650,#9473,#9474);
#7492=DIRECTION('axis',(0.,0.,1.));
#7493=DIRECTION('refdir',(1.,0.,0.));
#7494=DIRECTION('axis',(0.,0.,1.));
#7495=DIRECTION('refdir',(1.,0.,0.));
#7496=DIRECTION('axis',(0.,0.,1.));
#7497=DIRECTION('refdir',(1.,0.,0.));
#7498=DIRECTION('center_axis',(0.,0.,-1.));
#7499=DIRECTION('ref_axis',(0.,1.,0.));
#7500=DIRECTION('',(0.,1.,0.));
#7501=DIRECTION('',(1.,0.,0.));
#7502=DIRECTION('',(0.,-1.,0.));
#7503=DIRECTION('',(1.,0.,0.));
#7504=DIRECTION('center_axis',(0.,1.,-8.88178419700125E-16));
#7505=DIRECTION('ref_axis',(0.,8.88178419700125E-16,1.));
#7506=DIRECTION('',(0.,8.88178419700125E-16,1.));
#7507=DIRECTION('',(1.,0.,0.));
#7508=DIRECTION('',(0.,-8.88178419700125E-16,-1.));
#7509=DIRECTION('center_axis',(0.,-7.40148683083439E-16,-1.));
#7510=DIRECTION('ref_axis',(0.,1.,-7.40148683083439E-16));
#7511=DIRECTION('',(0.,1.,-7.40148683083439E-16));
#7512=DIRECTION('',(1.,0.,0.));
#7513=DIRECTION('',(0.,-1.,7.40148683083439E-16));
#7514=DIRECTION('center_axis',(0.,-0.707106781186547,-0.707106781186548));
#7515=DIRECTION('ref_axis',(0.,0.707106781186548,-0.707106781186547));
#7516=DIRECTION('',(0.,0.707106781186548,-0.707106781186547));
#7517=DIRECTION('',(1.,0.,0.));
#7518=DIRECTION('',(0.,-0.707106781186548,0.707106781186547));
#7519=DIRECTION('center_axis',(0.,-1.,2.77555756156289E-16));
#7520=DIRECTION('ref_axis',(0.,-2.77555756156289E-16,-1.));
#7521=DIRECTION('',(0.,-2.77555756156289E-16,-1.));
#7522=DIRECTION('',(1.,0.,0.));
#7523=DIRECTION('',(0.,2.77555756156289E-16,1.));
#7524=DIRECTION('center_axis',(0.,-0.707106781186547,0.707106781186548));
#7525=DIRECTION('ref_axis',(0.,-0.707106781186548,-0.707106781186547));
#7526=DIRECTION('',(0.,-0.707106781186548,-0.707106781186547));
#7527=DIRECTION('',(1.,0.,0.));
#7528=DIRECTION('',(0.,0.707106781186548,0.707106781186547));
#7529=DIRECTION('center_axis',(0.,7.40148683083438E-16,1.));
#7530=DIRECTION('ref_axis',(0.,-1.,7.40148683083438E-16));
#7531=DIRECTION('',(0.,-1.,7.40148683083438E-16));
#7532=DIRECTION('',(1.,0.,0.));
#7533=DIRECTION('',(0.,1.,-7.40148683083438E-16));
#7534=DIRECTION('center_axis',(0.,1.,-4.44089209850063E-16));
#7535=DIRECTION('ref_axis',(0.,4.44089209850063E-16,1.));
#7536=DIRECTION('',(0.,4.44089209850063E-16,1.));
#7537=DIRECTION('',(1.,0.,0.));
#7538=DIRECTION('',(0.,-4.44089209850063E-16,-1.));
#7539=DIRECTION('center_axis',(0.,2.41352831440251E-16,1.));
#7540=DIRECTION('ref_axis',(0.,-1.,2.41352831440251E-16));
#7541=DIRECTION('',(0.,-1.,2.41352831440251E-16));
#7542=DIRECTION('',(-1.,0.,0.));
#7543=DIRECTION('',(0.,1.,-2.41352831440251E-16));
#7544=DIRECTION('center_axis',(0.,-1.,2.41352831440251E-16));
#7545=DIRECTION('ref_axis',(0.,-2.41352831440251E-16,-1.));
#7546=DIRECTION('',(0.,-2.41352831440251E-16,-1.));
#7547=DIRECTION('',(1.,0.,0.));
#7548=DIRECTION('',(0.,2.41352831440251E-16,1.));
#7549=DIRECTION('',(1.,0.,0.));
#7550=DIRECTION('center_axis',(0.,0.,-1.));
#7551=DIRECTION('ref_axis',(0.,1.,0.));
#7552=DIRECTION('',(0.,1.,0.));
#7553=DIRECTION('',(1.,0.,0.));
#7554=DIRECTION('',(0.,-1.,0.));
#7555=DIRECTION('center_axis',(0.,-1.,0.));
#7556=DIRECTION('ref_axis',(0.,0.,-1.));
#7557=DIRECTION('',(0.,0.,-1.));
#7558=DIRECTION('',(1.,0.,0.));
#7559=DIRECTION('',(0.,0.,1.));
#7560=DIRECTION('center_axis',(0.,-0.707106781186547,0.707106781186548));
#7561=DIRECTION('ref_axis',(0.,-0.707106781186548,-0.707106781186547));
#7562=DIRECTION('',(0.,-0.707106781186548,-0.707106781186547));
#7563=DIRECTION('',(1.,0.,0.));
#7564=DIRECTION('',(0.,0.707106781186548,0.707106781186547));
#7565=DIRECTION('center_axis',(0.,0.,1.));
#7566=DIRECTION('ref_axis',(0.,-1.,0.));
#7567=DIRECTION('',(0.,-1.,0.));
#7568=DIRECTION('',(1.,0.,0.));
#7569=DIRECTION('',(0.,1.,0.));
#7570=DIRECTION('center_axis',(0.,0.707106781186548,0.707106781186547));
#7571=DIRECTION('ref_axis',(0.,-0.707106781186547,0.707106781186548));
#7572=DIRECTION('',(0.,-0.707106781186547,0.707106781186548));
#7573=DIRECTION('',(1.,0.,0.));
#7574=DIRECTION('',(0.,0.707106781186547,-0.707106781186548));
#7575=DIRECTION('center_axis',(0.,1.,0.));
#7576=DIRECTION('ref_axis',(0.,0.,1.));
#7577=DIRECTION('',(0.,0.,1.));
#7578=DIRECTION('',(1.,0.,0.));
#7579=DIRECTION('',(0.,0.,-1.));
#7580=DIRECTION('center_axis',(0.,0.,-1.));
#7581=DIRECTION('ref_axis',(0.,1.,0.));
#7582=DIRECTION('',(0.,1.,0.));
#7583=DIRECTION('',(1.,0.,0.));
#7584=DIRECTION('',(0.,-1.,0.));
#7585=DIRECTION('center_axis',(0.,1.,-2.41352831440251E-16));
#7586=DIRECTION('ref_axis',(0.,2.41352831440251E-16,1.));
#7587=DIRECTION('',(0.,2.41352831440251E-16,1.));
#7588=DIRECTION('',(-1.,0.,0.));
#7589=DIRECTION('',(0.,-2.41352831440251E-16,-1.));
#7590=DIRECTION('center_axis',(0.,0.,1.));
#7591=DIRECTION('ref_axis',(0.,-1.,0.));
#7592=DIRECTION('',(0.,-1.,0.));
#7593=DIRECTION('',(1.,0.,0.));
#7594=DIRECTION('',(0.,1.,0.));
#7595=DIRECTION('',(1.,0.,0.));
#7596=DIRECTION('center_axis',(0.,-1.,0.));
#7597=DIRECTION('ref_axis',(0.,0.,-1.));
#7598=DIRECTION('',(0.,0.,-1.));
#7599=DIRECTION('',(1.,0.,0.));
#7600=DIRECTION('',(0.,0.,1.));
#7601=DIRECTION('center_axis',(0.,0.,1.));
#7602=DIRECTION('ref_axis',(0.,-1.,0.));
#7603=DIRECTION('',(0.,-1.,0.));
#7604=DIRECTION('',(1.,0.,0.));
#7605=DIRECTION('',(0.,1.,0.));
#7606=DIRECTION('center_axis',(0.,0.707106781186548,0.707106781186548));
#7607=DIRECTION('ref_axis',(0.,-0.707106781186548,0.707106781186548));
#7608=DIRECTION('',(0.,-0.707106781186548,0.707106781186548));
#7609=DIRECTION('',(1.,0.,0.));
#7610=DIRECTION('',(0.,0.707106781186548,-0.707106781186548));
#7611=DIRECTION('center_axis',(0.,1.,0.));
#7612=DIRECTION('ref_axis',(0.,0.,1.));
#7613=DIRECTION('',(0.,0.,1.));
#7614=DIRECTION('',(1.,0.,0.));
#7615=DIRECTION('',(0.,0.,-1.));
#7616=DIRECTION('center_axis',(0.,0.707106781186548,-0.707106781186547));
#7617=DIRECTION('ref_axis',(0.,0.707106781186547,0.707106781186548));
#7618=DIRECTION('',(0.,0.707106781186547,0.707106781186548));
#7619=DIRECTION('',(1.,0.,0.));
#7620=DIRECTION('',(0.,-0.707106781186547,-0.707106781186548));
#7621=DIRECTION('center_axis',(0.,-7.40148683083438E-16,-1.));
#7622=DIRECTION('ref_axis',(0.,1.,-7.40148683083438E-16));
#7623=DIRECTION('',(0.,1.,-7.40148683083438E-16));
#7624=DIRECTION('',(1.,0.,0.));
#7625=DIRECTION('',(0.,-1.,7.40148683083438E-16));
#7626=DIRECTION('center_axis',(0.,-1.,0.));
#7627=DIRECTION('ref_axis',(0.,0.,-1.));
#7628=DIRECTION('',(0.,0.,-1.));
#7629=DIRECTION('',(1.,0.,0.));
#7630=DIRECTION('',(0.,0.,1.));
#7631=DIRECTION('center_axis',(0.,0.,-1.));
#7632=DIRECTION('ref_axis',(0.,1.,0.));
#7633=DIRECTION('',(0.,1.,0.));
#7634=DIRECTION('',(-1.,0.,0.));
#7635=DIRECTION('',(0.,-1.,0.));
#7636=DIRECTION('center_axis',(0.,1.,0.));
#7637=DIRECTION('ref_axis',(0.,0.,1.));
#7638=DIRECTION('',(0.,0.,1.));
#7639=DIRECTION('',(1.,0.,0.));
#7640=DIRECTION('',(0.,0.,-1.));
#7641=DIRECTION('',(1.,0.,0.));
#7642=DIRECTION('center_axis',(0.,0.,1.));
#7643=DIRECTION('ref_axis',(0.,-1.,0.));
#7644=DIRECTION('',(0.,-1.,0.));
#7645=DIRECTION('',(1.,0.,0.));
#7646=DIRECTION('',(0.,1.,0.));
#7647=DIRECTION('center_axis',(0.,1.,0.));
#7648=DIRECTION('ref_axis',(0.,0.,1.));
#7649=DIRECTION('',(0.,0.,1.));
#7650=DIRECTION('',(1.,0.,0.));
#7651=DIRECTION('',(0.,0.,-1.));
#7652=DIRECTION('center_axis',(0.,0.707106781186547,-0.707106781186548));
#7653=DIRECTION('ref_axis',(0.,0.707106781186548,0.707106781186547));
#7654=DIRECTION('',(0.,0.707106781186548,0.707106781186547));
#7655=DIRECTION('',(1.,0.,0.));
#7656=DIRECTION('',(0.,-0.707106781186548,-0.707106781186547));
#7657=DIRECTION('center_axis',(0.,0.,-1.));
#7658=DIRECTION('ref_axis',(0.,1.,0.));
#7659=DIRECTION('',(0.,1.,0.));
#7660=DIRECTION('',(1.,0.,0.));
#7661=DIRECTION('',(0.,-1.,0.));
#7662=DIRECTION('center_axis',(0.,-0.707106781186547,-0.707106781186548));
#7663=DIRECTION('ref_axis',(0.,0.707106781186548,-0.707106781186547));
#7664=DIRECTION('',(0.,0.707106781186548,-0.707106781186547));
#7665=DIRECTION('',(1.,0.,0.));
#7666=DIRECTION('',(0.,-0.707106781186548,0.707106781186547));
#7667=DIRECTION('center_axis',(0.,-1.,0.));
#7668=DIRECTION('ref_axis',(0.,0.,-1.));
#7669=DIRECTION('',(0.,0.,-1.));
#7670=DIRECTION('',(1.,0.,0.));
#7671=DIRECTION('',(0.,0.,1.));
#7672=DIRECTION('center_axis',(0.,0.,1.));
#7673=DIRECTION('ref_axis',(0.,-1.,0.));
#7674=DIRECTION('',(0.,-1.,0.));
#7675=DIRECTION('',(1.,0.,0.));
#7676=DIRECTION('',(0.,1.,0.));
#7677=DIRECTION('center_axis',(0.,-1.,0.));
#7678=DIRECTION('ref_axis',(0.,0.,-1.));
#7679=DIRECTION('',(0.,0.,-1.));
#7680=DIRECTION('',(-1.,0.,0.));
#7681=DIRECTION('',(0.,0.,1.));
#7682=DIRECTION('center_axis',(1.,0.,0.));
#7683=DIRECTION('ref_axis',(0.,0.,-1.));
#7684=DIRECTION('center_axis',(1.,0.,0.));
#7685=DIRECTION('ref_axis',(0.,0.,-1.));
#7686=DIRECTION('',(1.,0.,0.));
#7687=DIRECTION('center_axis',(-1.,0.,0.));
#7688=DIRECTION('ref_axis',(0.,0.,-1.));
#7689=DIRECTION('center_axis',(0.,1.,0.));
#7690=DIRECTION('ref_axis',(0.,0.,1.));
#7691=DIRECTION('',(0.,0.,1.));
#7692=DIRECTION('',(1.,0.,0.));
#7693=DIRECTION('',(0.,0.,1.));
#7694=DIRECTION('center_axis',(0.,1.,0.));
#7695=DIRECTION('ref_axis',(0.,0.,1.));
#7696=DIRECTION('',(0.,0.,1.));
#7697=DIRECTION('',(1.,0.,0.));
#7698=DIRECTION('',(0.,0.,1.));
#7699=DIRECTION('center_axis',(0.,0.,-1.));
#7700=DIRECTION('ref_axis',(0.,1.,0.));
#7701=DIRECTION('',(0.,1.,0.));
#7702=DIRECTION('',(0.,1.,0.));
#7703=DIRECTION('center_axis',(0.,0.,-1.));
#7704=DIRECTION('ref_axis',(0.,1.,0.));
#7705=DIRECTION('',(0.,1.,0.));
#7706=DIRECTION('',(1.,0.,0.));
#7707=DIRECTION('',(0.,1.,0.));
#7708=DIRECTION('center_axis',(0.,-1.,0.));
#7709=DIRECTION('ref_axis',(0.,0.,-1.));
#7710=DIRECTION('',(0.,0.,-1.));
#7711=DIRECTION('',(0.,0.,-1.));
#7712=DIRECTION('center_axis',(0.,-1.,0.));
#7713=DIRECTION('ref_axis',(0.,0.,-1.));
#7714=DIRECTION('',(0.,0.,-1.));
#7715=DIRECTION('',(1.,0.,0.));
#7716=DIRECTION('',(0.,0.,-1.));
#7717=DIRECTION('center_axis',(0.,0.,1.));
#7718=DIRECTION('ref_axis',(0.,-1.,0.));
#7719=DIRECTION('',(0.,-1.,0.));
#7720=DIRECTION('',(0.,-1.,0.));
#7721=DIRECTION('center_axis',(0.,0.,1.));
#7722=DIRECTION('ref_axis',(0.,-1.,0.));
#7723=DIRECTION('',(0.,-1.,0.));
#7724=DIRECTION('',(0.,-1.,0.));
#7725=DIRECTION('center_axis',(1.,0.,0.));
#7726=DIRECTION('ref_axis',(0.,0.,-1.));
#7727=DIRECTION('center_axis',(1.,0.,0.));
#7728=DIRECTION('ref_axis',(0.,0.,-1.));
#7729=DIRECTION('axis',(0.,0.,1.));
#7730=DIRECTION('refdir',(1.,0.,0.));
#7731=DIRECTION('center_axis',(0.,0.,1.));
#7732=DIRECTION('ref_axis',(1.,0.,0.));
#7733=DIRECTION('center_axis',(0.,0.,1.));
#7734=DIRECTION('ref_axis',(1.,0.,0.));
#7735=DIRECTION('',(0.,0.,1.));
#7736=DIRECTION('center_axis',(0.,0.,-1.));
#7737=DIRECTION('ref_axis',(1.,0.,0.));
#7738=DIRECTION('center_axis',(0.,0.,1.));
#7739=DIRECTION('ref_axis',(1.,0.,0.));
#7740=DIRECTION('center_axis',(0.,0.,1.));
#7741=DIRECTION('ref_axis',(1.,0.,0.));
#7742=DIRECTION('',(0.,0.,1.));
#7743=DIRECTION('center_axis',(0.,0.,-1.));
#7744=DIRECTION('ref_axis',(1.,0.,0.));
#7745=DIRECTION('center_axis',(0.,0.,1.));
#7746=DIRECTION('ref_axis',(1.,0.,0.));
#7747=DIRECTION('center_axis',(0.,0.,1.));
#7748=DIRECTION('ref_axis',(1.,0.,0.));
#7749=DIRECTION('',(0.,0.,1.));
#7750=DIRECTION('center_axis',(0.,0.,-1.));
#7751=DIRECTION('ref_axis',(1.,0.,0.));
#7752=DIRECTION('center_axis',(0.,0.,1.));
#7753=DIRECTION('ref_axis',(1.,0.,0.));
#7754=DIRECTION('center_axis',(0.,0.,1.));
#7755=DIRECTION('ref_axis',(1.,0.,0.));
#7756=DIRECTION('',(0.,0.,1.));
#7757=DIRECTION('center_axis',(0.,0.,-1.));
#7758=DIRECTION('ref_axis',(1.,0.,0.));
#7759=DIRECTION('center_axis',(0.,0.,1.));
#7760=DIRECTION('ref_axis',(1.,0.,0.));
#7761=DIRECTION('center_axis',(0.,0.,1.));
#7762=DIRECTION('ref_axis',(1.,0.,0.));
#7763=DIRECTION('',(0.,0.,1.));
#7764=DIRECTION('center_axis',(0.,0.,-1.));
#7765=DIRECTION('ref_axis',(1.,0.,0.));
#7766=DIRECTION('center_axis',(0.,0.,1.));
#7767=DIRECTION('ref_axis',(1.,0.,0.));
#7768=DIRECTION('center_axis',(0.,0.,1.));
#7769=DIRECTION('ref_axis',(1.,0.,0.));
#7770=DIRECTION('',(0.,0.,1.));
#7771=DIRECTION('center_axis',(0.,0.,-1.));
#7772=DIRECTION('ref_axis',(1.,0.,0.));
#7773=DIRECTION('center_axis',(0.,0.,1.));
#7774=DIRECTION('ref_axis',(1.,0.,0.));
#7775=DIRECTION('center_axis',(0.,0.,1.));
#7776=DIRECTION('ref_axis',(1.,0.,0.));
#7777=DIRECTION('',(0.,0.,1.));
#7778=DIRECTION('center_axis',(0.,0.,-1.));
#7779=DIRECTION('ref_axis',(1.,0.,0.));
#7780=DIRECTION('center_axis',(0.,0.,1.));
#7781=DIRECTION('ref_axis',(1.,0.,0.));
#7782=DIRECTION('center_axis',(0.,0.,1.));
#7783=DIRECTION('ref_axis',(1.,0.,0.));
#7784=DIRECTION('',(0.,0.,1.));
#7785=DIRECTION('center_axis',(0.,0.,-1.));
#7786=DIRECTION('ref_axis',(1.,0.,0.));
#7787=DIRECTION('center_axis',(0.,0.,1.));
#7788=DIRECTION('ref_axis',(1.,0.,0.));
#7789=DIRECTION('center_axis',(0.,0.,1.));
#7790=DIRECTION('ref_axis',(1.,0.,0.));
#7791=DIRECTION('',(0.,0.,1.));
#7792=DIRECTION('center_axis',(0.,0.,-1.));
#7793=DIRECTION('ref_axis',(1.,0.,0.));
#7794=DIRECTION('center_axis',(0.,0.,1.));
#7795=DIRECTION('ref_axis',(1.,0.,0.));
#7796=DIRECTION('center_axis',(0.,0.,1.));
#7797=DIRECTION('ref_axis',(1.,0.,0.));
#7798=DIRECTION('',(0.,0.,1.));
#7799=DIRECTION('center_axis',(0.,0.,-1.));
#7800=DIRECTION('ref_axis',(1.,0.,0.));
#7801=DIRECTION('center_axis',(0.,0.,1.));
#7802=DIRECTION('ref_axis',(1.,0.,0.));
#7803=DIRECTION('center_axis',(0.,0.,1.));
#7804=DIRECTION('ref_axis',(1.,0.,0.));
#7805=DIRECTION('',(0.,0.,1.));
#7806=DIRECTION('center_axis',(0.,0.,-1.));
#7807=DIRECTION('ref_axis',(1.,0.,0.));
#7808=DIRECTION('center_axis',(0.,0.,1.));
#7809=DIRECTION('ref_axis',(1.,0.,0.));
#7810=DIRECTION('center_axis',(0.,0.,1.));
#7811=DIRECTION('ref_axis',(1.,0.,0.));
#7812=DIRECTION('',(0.,0.,1.));
#7813=DIRECTION('center_axis',(0.,0.,-1.));
#7814=DIRECTION('ref_axis',(1.,0.,0.));
#7815=DIRECTION('center_axis',(0.,1.,0.));
#7816=DIRECTION('ref_axis',(-1.,0.,0.));
#7817=DIRECTION('',(-1.,0.,0.));
#7818=DIRECTION('',(0.,0.,1.));
#7819=DIRECTION('',(-1.,0.,0.));
#7820=DIRECTION('',(0.,0.,1.));
#7821=DIRECTION('center_axis',(1.,0.,0.));
#7822=DIRECTION('ref_axis',(0.,1.,0.));
#7823=DIRECTION('',(0.,1.,0.));
#7824=DIRECTION('',(0.,1.,0.));
#7825=DIRECTION('',(0.,0.,1.));
#7826=DIRECTION('center_axis',(0.,-1.,0.));
#7827=DIRECTION('ref_axis',(1.,0.,0.));
#7828=DIRECTION('',(1.,0.,0.));
#7829=DIRECTION('',(1.,0.,0.));
#7830=DIRECTION('',(0.,0.,1.));
#7831=DIRECTION('center_axis',(-1.,0.,0.));
#7832=DIRECTION('ref_axis',(0.,-1.,0.));
#7833=DIRECTION('',(0.,-1.,0.));
#7834=DIRECTION('',(0.,-1.,0.));
#7835=DIRECTION('center_axis',(0.,0.,1.));
#7836=DIRECTION('ref_axis',(1.,0.,0.));
#7837=DIRECTION('center_axis',(0.,0.,1.));
#7838=DIRECTION('ref_axis',(1.,0.,0.));
#7839=DIRECTION('axis',(0.,0.,1.));
#7840=DIRECTION('refdir',(1.,0.,0.));
#7841=DIRECTION('center_axis',(0.,0.,1.));
#7842=DIRECTION('ref_axis',(1.,0.,0.));
#7843=DIRECTION('',(1.,0.,0.));
#7844=DIRECTION('',(0.,-1.,0.));
#7845=DIRECTION('',(-1.,0.,0.));
#7846=DIRECTION('',(0.,1.,0.));
#7847=DIRECTION('center_axis',(0.,1.,0.));
#7848=DIRECTION('ref_axis',(-1.,0.,0.));
#7849=DIRECTION('',(0.,0.,1.));
#7850=DIRECTION('',(-1.,0.,0.));
#7851=DIRECTION('',(0.,0.,1.));
#7852=DIRECTION('center_axis',(0.,0.,1.));
#7853=DIRECTION('ref_axis',(1.,0.,0.));
#7854=DIRECTION('',(0.,-1.,0.));
#7855=DIRECTION('',(1.,0.,0.));
#7856=DIRECTION('',(0.,1.,0.));
#7857=DIRECTION('center_axis',(0.,0.,-1.));
#7858=DIRECTION('ref_axis',(1.,0.,0.));
#7859=DIRECTION('center_axis',(-1.,0.,0.));
#7860=DIRECTION('ref_axis',(0.,-1.,0.));
#7861=DIRECTION('',(0.,0.,1.));
#7862=DIRECTION('',(0.,0.707106781186548,0.707106781186548));
#7863=DIRECTION('',(0.,-1.,0.));
#7864=DIRECTION('',(0.,0.707106781186548,-0.707106781186548));
#7865=DIRECTION('',(0.,0.,1.));
#7866=DIRECTION('',(0.,-1.,0.));
#7867=DIRECTION('',(0.,0.,1.));
#7868=DIRECTION('center_axis',(0.,-1.,0.));
#7869=DIRECTION('ref_axis',(1.,0.,0.));
#7870=DIRECTION('',(1.,0.,0.));
#7871=DIRECTION('',(0.,0.,1.));
#7872=DIRECTION('center_axis',(0.,0.,1.));
#7873=DIRECTION('ref_axis',(1.,0.,0.));
#7874=DIRECTION('',(-1.,0.,0.));
#7875=DIRECTION('',(0.,1.,0.));
#7876=DIRECTION('center_axis',(1.,0.,0.));
#7877=DIRECTION('ref_axis',(0.,1.,0.));
#7878=DIRECTION('',(0.,0.,1.));
#7879=DIRECTION('',(0.,-0.707106781186548,0.707106781186548));
#7880=DIRECTION('',(0.,1.,0.));
#7881=DIRECTION('',(0.,-0.707106781186548,-0.707106781186548));
#7882=DIRECTION('',(0.,0.,1.));
#7883=DIRECTION('center_axis',(0.,-1.,0.));
#7884=DIRECTION('ref_axis',(1.,0.,0.));
#7885=DIRECTION('',(-1.,0.,0.));
#7886=DIRECTION('center_axis',(0.,-0.707106781186548,-0.707106781186548));
#7887=DIRECTION('ref_axis',(-1.,0.,0.));
#7888=DIRECTION('',(1.,0.,0.));
#7889=DIRECTION('center_axis',(0.,0.707106781186548,0.707106781186548));
#7890=DIRECTION('ref_axis',(0.,0.707106781186547,-0.707106781186547));
#7891=DIRECTION('',(1.,0.,0.));
#7892=DIRECTION('center_axis',(0.,0.,1.));
#7893=DIRECTION('ref_axis',(1.,0.,0.));
#7894=DIRECTION('center_axis',(0.,0.,-1.));
#7895=DIRECTION('ref_axis',(1.,0.,0.));
#7896=DIRECTION('',(0.,0.,1.));
#7897=DIRECTION('center_axis',(0.,0.,-1.));
#7898=DIRECTION('ref_axis',(1.,0.,0.));
#7899=DIRECTION('center_axis',(0.,-0.707106781186548,0.707106781186548));
#7900=DIRECTION('ref_axis',(0.,0.707106781186547,0.707106781186547));
#7901=DIRECTION('center_axis',(0.,0.,-1.));
#7902=DIRECTION('ref_axis',(1.,0.,0.));
#7903=DIRECTION('center_axis',(0.,0.,1.));
#7904=DIRECTION('ref_axis',(1.,0.,0.));
#7905=DIRECTION('',(-1.,0.,0.));
#7906=DIRECTION('center_axis',(0.,0.,1.));
#7907=DIRECTION('ref_axis',(1.,0.,0.));
#7908=DIRECTION('',(-1.,0.,0.));
#7909=DIRECTION('center_axis',(0.,0.707106781186548,-0.707106781186548));
#7910=DIRECTION('ref_axis',(-1.,0.,0.));
#7911=DIRECTION('',(1.,0.,0.));
#7912=DIRECTION('center_axis',(0.,1.,0.));
#7913=DIRECTION('ref_axis',(-1.,0.,0.));
#7914=DIRECTION('axis',(0.,0.,1.));
#7915=DIRECTION('refdir',(1.,0.,0.));
#7916=DIRECTION('center_axis',(0.,1.,0.));
#7917=DIRECTION('ref_axis',(1.,0.,0.));
#7918=DIRECTION('center_axis',(0.,1.,0.));
#7919=DIRECTION('ref_axis',(1.,0.,0.));
#7920=DIRECTION('',(0.707106781186548,-0.707106781186547,-8.65956056235494E-17));
#7921=DIRECTION('center_axis',(0.,-1.,0.));
#7922=DIRECTION('ref_axis',(1.,0.,0.));
#7923=DIRECTION('center_axis',(0.,1.,0.));
#7924=DIRECTION('ref_axis',(1.,0.,0.));
#7925=DIRECTION('',(0.,-1.,0.));
#7926=DIRECTION('center_axis',(0.,-1.,0.));
#7927=DIRECTION('ref_axis',(1.,0.,0.));
#7928=DIRECTION('center_axis',(0.,1.,0.));
#7929=DIRECTION('ref_axis',(1.,0.,0.));
#7930=DIRECTION('center_axis',(0.,1.,0.));
#7931=DIRECTION('ref_axis',(1.,0.,0.));
#7932=DIRECTION('center_axis',(0.,1.,0.));
#7933=DIRECTION('ref_axis',(1.,0.,0.));
#7934=DIRECTION('',(0.,-1.,0.));
#7935=DIRECTION('center_axis',(0.,1.,0.));
#7936=DIRECTION('ref_axis',(1.,0.,0.));
#7937=DIRECTION('center_axis',(0.,1.,0.));
#7938=DIRECTION('ref_axis',(1.,0.,0.));
#7939=DIRECTION('axis',(0.,0.,1.));
#7940=DIRECTION('refdir',(1.,0.,0.));
#7941=DIRECTION('center_axis',(0.,1.,0.));
#7942=DIRECTION('ref_axis',(-1.,0.,0.));
#7943=DIRECTION('',(-1.,0.,0.));
#7944=DIRECTION('',(0.,0.,1.));
#7945=DIRECTION('',(-1.,0.,0.));
#7946=DIRECTION('',(0.,0.,1.));
#7947=DIRECTION('center_axis',(1.,0.,0.));
#7948=DIRECTION('ref_axis',(0.,1.,0.));
#7949=DIRECTION('',(0.,1.,0.));
#7950=DIRECTION('',(0.,1.,0.));
#7951=DIRECTION('',(0.,0.,1.));
#7952=DIRECTION('center_axis',(0.,-1.,0.));
#7953=DIRECTION('ref_axis',(1.,0.,0.));
#7954=DIRECTION('',(1.,0.,0.));
#7955=DIRECTION('',(1.,0.,0.));
#7956=DIRECTION('',(0.,0.,1.));
#7957=DIRECTION('center_axis',(-1.,0.,0.));
#7958=DIRECTION('ref_axis',(0.,-1.,0.));
#7959=DIRECTION('',(0.,-1.,0.));
#7960=DIRECTION('',(0.,-1.,0.));
#7961=DIRECTION('center_axis',(0.,0.,1.));
#7962=DIRECTION('ref_axis',(1.,0.,0.));
#7963=DIRECTION('center_axis',(0.,0.,1.));
#7964=DIRECTION('ref_axis',(1.,0.,0.));
#7965=DIRECTION('axis',(0.,0.,1.));
#7966=DIRECTION('refdir',(1.,0.,0.));
#7967=DIRECTION('center_axis',(0.,1.,0.));
#7968=DIRECTION('ref_axis',(-1.,0.,0.));
#7969=DIRECTION('',(-1.,0.,0.));
#7970=DIRECTION('',(0.,0.,1.));
#7971=DIRECTION('',(-1.,0.,0.));
#7972=DIRECTION('',(0.,0.,1.));
#7973=DIRECTION('center_axis',(1.,0.,0.));
#7974=DIRECTION('ref_axis',(0.,1.,0.));
#7975=DIRECTION('',(0.,1.,0.));
#7976=DIRECTION('',(0.,1.,0.));
#7977=DIRECTION('',(0.,0.,1.));
#7978=DIRECTION('center_axis',(0.,-1.,0.));
#7979=DIRECTION('ref_axis',(1.,0.,0.));
#7980=DIRECTION('',(1.,0.,0.));
#7981=DIRECTION('',(1.,0.,0.));
#7982=DIRECTION('',(0.,0.,1.));
#7983=DIRECTION('center_axis',(-1.,0.,0.));
#7984=DIRECTION('ref_axis',(0.,-1.,0.));
#7985=DIRECTION('',(0.,-1.,0.));
#7986=DIRECTION('',(0.,-1.,0.));
#7987=DIRECTION('center_axis',(0.,0.,1.));
#7988=DIRECTION('ref_axis',(1.,0.,0.));
#7989=DIRECTION('center_axis',(0.,0.,1.));
#7990=DIRECTION('ref_axis',(1.,0.,0.));
#7991=DIRECTION('axis',(0.,0.,1.));
#7992=DIRECTION('refdir',(1.,0.,0.));
#7993=DIRECTION('center_axis',(0.,0.,1.));
#7994=DIRECTION('ref_axis',(1.,0.,0.));
#7995=DIRECTION('center_axis',(0.,0.,1.));
#7996=DIRECTION('ref_axis',(1.,0.,0.));
#7997=DIRECTION('',(0.,0.,1.));
#7998=DIRECTION('center_axis',(0.,0.,-1.));
#7999=DIRECTION('ref_axis',(1.,0.,0.));
#8000=DIRECTION('center_axis',(0.,0.,1.));
#8001=DIRECTION('ref_axis',(1.,0.,0.));
#8002=DIRECTION('center_axis',(0.,0.,1.));
#8003=DIRECTION('ref_axis',(1.,0.,0.));
#8004=DIRECTION('',(0.,0.,1.));
#8005=DIRECTION('center_axis',(0.,0.,-1.));
#8006=DIRECTION('ref_axis',(1.,0.,0.));
#8007=DIRECTION('center_axis',(0.,1.,0.));
#8008=DIRECTION('ref_axis',(1.,0.,0.));
#8009=DIRECTION('center_axis',(0.,1.,0.));
#8010=DIRECTION('ref_axis',(1.,0.,0.));
#8011=DIRECTION('',(0.,-1.,0.));
#8012=DIRECTION('center_axis',(0.,-1.,0.));
#8013=DIRECTION('ref_axis',(1.,0.,0.));
#8014=DIRECTION('',(0.,1.,0.));
#8015=DIRECTION('center_axis',(0.,1.,0.));
#8016=DIRECTION('ref_axis',(-1.,0.,0.));
#8017=DIRECTION('',(-1.,0.,0.));
#8018=DIRECTION('',(0.,0.,1.));
#8019=DIRECTION('',(-1.,0.,0.));
#8020=DIRECTION('',(0.,0.,1.));
#8021=DIRECTION('',(-1.,0.,0.));
#8022=DIRECTION('center_axis',(0.,-1.,0.));
#8023=DIRECTION('ref_axis',(1.,0.,0.));
#8024=DIRECTION('center_axis',(0.,-1.,0.));
#8025=DIRECTION('ref_axis',(1.,0.,0.));
#8026=DIRECTION('center_axis',(0.,0.,1.));
#8027=DIRECTION('ref_axis',(1.,0.,0.));
#8028=DIRECTION('',(1.,0.,0.));
#8029=DIRECTION('',(0.,1.,0.));
#8030=DIRECTION('center_axis',(0.,1.,0.));
#8031=DIRECTION('ref_axis',(1.,0.,0.));
#8032=DIRECTION('center_axis',(0.,1.,0.));
#8033=DIRECTION('ref_axis',(1.,0.,0.));
#8034=DIRECTION('',(0.,1.,0.));
#8035=DIRECTION('center_axis',(0.,1.,0.));
#8036=DIRECTION('ref_axis',(1.,0.,0.));
#8037=DIRECTION('center_axis',(0.,1.,0.));
#8038=DIRECTION('ref_axis',(1.,0.,0.));
#8039=DIRECTION('',(0.,1.,0.));
#8040=DIRECTION('center_axis',(0.,0.,1.));
#8041=DIRECTION('ref_axis',(1.,0.,0.));
#8042=DIRECTION('',(-1.,0.,0.));
#8043=DIRECTION('',(0.,1.,0.));
#8044=DIRECTION('',(1.,0.,0.));
#8045=DIRECTION('',(0.,1.,0.));
#8046=DIRECTION('center_axis',(0.,1.,0.));
#8047=DIRECTION('ref_axis',(1.,0.,0.));
#8048=DIRECTION('',(0.,0.,-1.));
#8049=DIRECTION('',(1.,0.,0.));
#8050=DIRECTION('',(0.,0.,1.));
#8051=DIRECTION('center_axis',(1.,0.,0.));
#8052=DIRECTION('ref_axis',(0.,1.,0.));
#8053=DIRECTION('',(0.,1.,0.));
#8054=DIRECTION('',(0.,0.,1.));
#8055=DIRECTION('center_axis',(0.,-1.,0.));
#8056=DIRECTION('ref_axis',(1.,0.,0.));
#8057=DIRECTION('',(1.,0.,0.));
#8058=DIRECTION('',(0.,0.,1.));
#8059=DIRECTION('center_axis',(-1.,0.,0.));
#8060=DIRECTION('ref_axis',(0.,-1.,0.));
#8061=DIRECTION('',(0.,-1.,0.));
#8062=DIRECTION('',(0.,-1.,0.));
#8063=DIRECTION('center_axis',(0.,0.,1.));
#8064=DIRECTION('ref_axis',(1.,0.,0.));
#8065=DIRECTION('center_axis',(0.,0.,1.));
#8066=DIRECTION('ref_axis',(1.,0.,0.));
#8067=DIRECTION('axis',(0.,0.,1.));
#8068=DIRECTION('refdir',(1.,0.,0.));
#8069=DIRECTION('center_axis',(0.,1.,0.));
#8070=DIRECTION('ref_axis',(1.,0.,0.));
#8071=DIRECTION('center_axis',(0.,1.,0.));
#8072=DIRECTION('ref_axis',(1.,0.,0.));
#8073=DIRECTION('',(0.,1.,0.));
#8074=DIRECTION('center_axis',(0.,-1.,0.));
#8075=DIRECTION('ref_axis',(1.,0.,0.));
#8076=DIRECTION('center_axis',(0.,1.,0.));
#8077=DIRECTION('ref_axis',(1.,0.,0.));
#8078=DIRECTION('center_axis',(0.,1.,0.));
#8079=DIRECTION('ref_axis',(1.,0.,0.));
#8080=DIRECTION('center_axis',(0.,1.,0.));
#8081=DIRECTION('ref_axis',(1.,0.,0.));
#8082=DIRECTION('center_axis',(0.,1.,0.));
#8083=DIRECTION('ref_axis',(1.,0.,0.));
#8084=DIRECTION('center_axis',(0.,1.,0.));
#8085=DIRECTION('ref_axis',(1.,0.,0.));
#8086=DIRECTION('',(0.,-1.,0.));
#8087=DIRECTION('center_axis',(0.,1.,0.));
#8088=DIRECTION('ref_axis',(1.,0.,0.));
#8089=DIRECTION('center_axis',(0.,1.,0.));
#8090=DIRECTION('ref_axis',(1.,0.,0.));
#8091=DIRECTION('center_axis',(0.,1.,0.));
#8092=DIRECTION('ref_axis',(1.,0.,0.));
#8093=DIRECTION('center_axis',(0.,1.,0.));
#8094=DIRECTION('ref_axis',(1.,0.,0.));
#8095=DIRECTION('',(0.,-1.,0.));
#8096=DIRECTION('center_axis',(0.,1.,0.));
#8097=DIRECTION('ref_axis',(1.,0.,0.));
#8098=DIRECTION('axis',(0.,0.,1.));
#8099=DIRECTION('refdir',(1.,0.,0.));
#8100=DIRECTION('center_axis',(0.,1.,0.));
#8101=DIRECTION('ref_axis',(1.,0.,0.));
#8102=DIRECTION('center_axis',(0.,-1.,0.));
#8103=DIRECTION('ref_axis',(1.,0.,0.));
#8104=DIRECTION('',(0.,-1.,0.));
#8105=DIRECTION('center_axis',(0.,-1.,0.));
#8106=DIRECTION('ref_axis',(1.,0.,0.));
#8107=DIRECTION('center_axis',(0.,1.,0.));
#8108=DIRECTION('ref_axis',(1.,0.,0.));
#8109=DIRECTION('center_axis',(0.,1.,0.));
#8110=DIRECTION('ref_axis',(1.,0.,0.));
#8111=DIRECTION('',(0.,-1.,0.));
#8112=DIRECTION('center_axis',(0.,1.,0.));
#8113=DIRECTION('ref_axis',(1.,0.,0.));
#8114=DIRECTION('center_axis',(0.,1.,0.));
#8115=DIRECTION('ref_axis',(1.,0.,0.));
#8116=DIRECTION('center_axis',(0.,1.,0.));
#8117=DIRECTION('ref_axis',(1.,0.,0.));
#8118=DIRECTION('axis',(0.,0.,1.));
#8119=DIRECTION('refdir',(1.,0.,0.));
#8120=DIRECTION('center_axis',(0.,1.,0.));
#8121=DIRECTION('ref_axis',(1.,0.,0.));
#8122=DIRECTION('center_axis',(0.,-1.,0.));
#8123=DIRECTION('ref_axis',(1.,0.,0.));
#8124=DIRECTION('',(0.,-1.,0.));
#8125=DIRECTION('center_axis',(0.,-1.,0.));
#8126=DIRECTION('ref_axis',(1.,0.,0.));
#8127=DIRECTION('center_axis',(0.,1.,0.));
#8128=DIRECTION('ref_axis',(1.,0.,0.));
#8129=DIRECTION('center_axis',(0.,1.,0.));
#8130=DIRECTION('ref_axis',(1.,0.,0.));
#8131=DIRECTION('',(0.,-1.,0.));
#8132=DIRECTION('center_axis',(0.,1.,0.));
#8133=DIRECTION('ref_axis',(1.,0.,0.));
#8134=DIRECTION('center_axis',(0.,1.,0.));
#8135=DIRECTION('ref_axis',(1.,0.,0.));
#8136=DIRECTION('center_axis',(0.,1.,0.));
#8137=DIRECTION('ref_axis',(1.,0.,0.));
#8138=DIRECTION('axis',(0.,0.,1.));
#8139=DIRECTION('refdir',(1.,0.,0.));
#8140=DIRECTION('center_axis',(0.,1.,0.));
#8141=DIRECTION('ref_axis',(1.,0.,0.));
#8142=DIRECTION('center_axis',(0.,-1.,0.));
#8143=DIRECTION('ref_axis',(1.,0.,0.));
#8144=DIRECTION('',(0.,-1.,0.));
#8145=DIRECTION('center_axis',(0.,-1.,0.));
#8146=DIRECTION('ref_axis',(1.,0.,0.));
#8147=DIRECTION('center_axis',(0.,1.,0.));
#8148=DIRECTION('ref_axis',(1.,0.,0.));
#8149=DIRECTION('center_axis',(0.,1.,0.));
#8150=DIRECTION('ref_axis',(1.,0.,0.));
#8151=DIRECTION('',(0.,-1.,0.));
#8152=DIRECTION('center_axis',(0.,1.,0.));
#8153=DIRECTION('ref_axis',(1.,0.,0.));
#8154=DIRECTION('center_axis',(0.,1.,0.));
#8155=DIRECTION('ref_axis',(1.,0.,0.));
#8156=DIRECTION('center_axis',(0.,1.,0.));
#8157=DIRECTION('ref_axis',(1.,0.,0.));
#8158=DIRECTION('axis',(0.,0.,1.));
#8159=DIRECTION('refdir',(1.,0.,0.));
#8160=DIRECTION('center_axis',(0.,1.,0.));
#8161=DIRECTION('ref_axis',(1.,0.,0.));
#8162=DIRECTION('center_axis',(0.,1.,0.));
#8163=DIRECTION('ref_axis',(1.,0.,0.));
#8164=DIRECTION('',(0.,1.,0.));
#8165=DIRECTION('center_axis',(0.,-1.,0.));
#8166=DIRECTION('ref_axis',(1.,0.,0.));
#8167=DIRECTION('center_axis',(0.,1.,0.));
#8168=DIRECTION('ref_axis',(1.,0.,0.));
#8169=DIRECTION('center_axis',(0.,1.,0.));
#8170=DIRECTION('ref_axis',(1.,0.,0.));
#8171=DIRECTION('center_axis',(0.,1.,0.));
#8172=DIRECTION('ref_axis',(1.,0.,0.));
#8173=DIRECTION('center_axis',(0.,1.,0.));
#8174=DIRECTION('ref_axis',(1.,0.,0.));
#8175=DIRECTION('center_axis',(0.,1.,0.));
#8176=DIRECTION('ref_axis',(1.,0.,0.));
#8177=DIRECTION('',(0.,-1.,0.));
#8178=DIRECTION('center_axis',(0.,1.,0.));
#8179=DIRECTION('ref_axis',(1.,0.,0.));
#8180=DIRECTION('center_axis',(0.,1.,0.));
#8181=DIRECTION('ref_axis',(1.,0.,0.));
#8182=DIRECTION('center_axis',(0.,1.,0.));
#8183=DIRECTION('ref_axis',(1.,0.,0.));
#8184=DIRECTION('center_axis',(0.,1.,0.));
#8185=DIRECTION('ref_axis',(1.,0.,0.));
#8186=DIRECTION('',(0.,-1.,0.));
#8187=DIRECTION('center_axis',(0.,1.,0.));
#8188=DIRECTION('ref_axis',(1.,0.,0.));
#8189=DIRECTION('axis',(0.,0.,1.));
#8190=DIRECTION('refdir',(1.,0.,0.));
#8191=DIRECTION('center_axis',(0.,1.,0.));
#8192=DIRECTION('ref_axis',(1.,0.,0.));
#8193=DIRECTION('center_axis',(0.,-1.,0.));
#8194=DIRECTION('ref_axis',(1.,0.,0.));
#8195=DIRECTION('',(0.,-1.,0.));
#8196=DIRECTION('center_axis',(0.,-1.,0.));
#8197=DIRECTION('ref_axis',(1.,0.,0.));
#8198=DIRECTION('center_axis',(0.,1.,0.));
#8199=DIRECTION('ref_axis',(1.,0.,0.));
#8200=DIRECTION('center_axis',(0.,1.,0.));
#8201=DIRECTION('ref_axis',(1.,0.,0.));
#8202=DIRECTION('',(0.,-1.,0.));
#8203=DIRECTION('center_axis',(0.,1.,0.));
#8204=DIRECTION('ref_axis',(1.,0.,0.));
#8205=DIRECTION('center_axis',(0.,1.,0.));
#8206=DIRECTION('ref_axis',(1.,0.,0.));
#8207=DIRECTION('center_axis',(0.,1.,0.));
#8208=DIRECTION('ref_axis',(1.,0.,0.));
#8209=DIRECTION('axis',(0.,0.,1.));
#8210=DIRECTION('refdir',(1.,0.,0.));
#8211=DIRECTION('center_axis',(0.,1.,0.));
#8212=DIRECTION('ref_axis',(1.,0.,0.));
#8213=DIRECTION('center_axis',(0.,-1.,0.));
#8214=DIRECTION('ref_axis',(1.,0.,0.));
#8215=DIRECTION('',(0.,-1.,0.));
#8216=DIRECTION('center_axis',(0.,-1.,0.));
#8217=DIRECTION('ref_axis',(1.,0.,0.));
#8218=DIRECTION('center_axis',(0.,1.,0.));
#8219=DIRECTION('ref_axis',(1.,0.,0.));
#8220=DIRECTION('center_axis',(0.,1.,0.));
#8221=DIRECTION('ref_axis',(1.,0.,0.));
#8222=DIRECTION('',(0.,-1.,0.));
#8223=DIRECTION('center_axis',(0.,1.,0.));
#8224=DIRECTION('ref_axis',(1.,0.,0.));
#8225=DIRECTION('center_axis',(0.,1.,0.));
#8226=DIRECTION('ref_axis',(1.,0.,0.));
#8227=DIRECTION('center_axis',(0.,1.,0.));
#8228=DIRECTION('ref_axis',(1.,0.,0.));
#8229=DIRECTION('axis',(0.,0.,1.));
#8230=DIRECTION('refdir',(1.,0.,0.));
#8231=DIRECTION('center_axis',(0.,0.,1.));
#8232=DIRECTION('ref_axis',(1.,0.,0.));
#8233=DIRECTION('center_axis',(0.,0.,1.));
#8234=DIRECTION('ref_axis',(1.,0.,0.));
#8235=DIRECTION('',(0.,0.,1.));
#8236=DIRECTION('center_axis',(0.,0.,-1.));
#8237=DIRECTION('ref_axis',(1.,0.,0.));
#8238=DIRECTION('center_axis',(0.,0.,1.));
#8239=DIRECTION('ref_axis',(1.,0.,0.));
#8240=DIRECTION('center_axis',(0.,0.,1.));
#8241=DIRECTION('ref_axis',(1.,0.,0.));
#8242=DIRECTION('',(0.,0.,1.));
#8243=DIRECTION('center_axis',(0.,0.,-1.));
#8244=DIRECTION('ref_axis',(1.,0.,0.));
#8245=DIRECTION('center_axis',(0.,1.,0.));
#8246=DIRECTION('ref_axis',(1.,0.,0.));
#8247=DIRECTION('center_axis',(0.,1.,0.));
#8248=DIRECTION('ref_axis',(1.,0.,0.));
#8249=DIRECTION('',(0.,-1.,0.));
#8250=DIRECTION('center_axis',(0.,-1.,0.));
#8251=DIRECTION('ref_axis',(1.,0.,0.));
#8252=DIRECTION('',(0.,1.,0.));
#8253=DIRECTION('center_axis',(0.,1.,0.));
#8254=DIRECTION('ref_axis',(-1.,0.,0.));
#8255=DIRECTION('',(-1.,0.,0.));
#8256=DIRECTION('',(0.,0.,1.));
#8257=DIRECTION('',(-1.,0.,0.));
#8258=DIRECTION('',(0.,0.,1.));
#8259=DIRECTION('',(-1.,0.,0.));
#8260=DIRECTION('center_axis',(0.,-1.,0.));
#8261=DIRECTION('ref_axis',(1.,0.,0.));
#8262=DIRECTION('center_axis',(0.,-1.,0.));
#8263=DIRECTION('ref_axis',(1.,0.,0.));
#8264=DIRECTION('center_axis',(0.,0.,1.));
#8265=DIRECTION('ref_axis',(1.,0.,0.));
#8266=DIRECTION('',(1.,0.,0.));
#8267=DIRECTION('',(0.,1.,0.));
#8268=DIRECTION('center_axis',(0.,1.,0.));
#8269=DIRECTION('ref_axis',(1.,0.,0.));
#8270=DIRECTION('center_axis',(0.,1.,0.));
#8271=DIRECTION('ref_axis',(1.,0.,0.));
#8272=DIRECTION('',(0.,1.,0.));
#8273=DIRECTION('center_axis',(0.,1.,0.));
#8274=DIRECTION('ref_axis',(1.,0.,0.));
#8275=DIRECTION('center_axis',(0.,1.,0.));
#8276=DIRECTION('ref_axis',(1.,0.,0.));
#8277=DIRECTION('',(0.,1.,0.));
#8278=DIRECTION('center_axis',(0.,0.,1.));
#8279=DIRECTION('ref_axis',(1.,0.,0.));
#8280=DIRECTION('',(-1.,0.,0.));
#8281=DIRECTION('',(0.,1.,0.));
#8282=DIRECTION('',(1.,0.,0.));
#8283=DIRECTION('',(0.,1.,0.));
#8284=DIRECTION('center_axis',(0.,1.,0.));
#8285=DIRECTION('ref_axis',(1.,0.,0.));
#8286=DIRECTION('',(0.,0.,-1.));
#8287=DIRECTION('',(1.,0.,0.));
#8288=DIRECTION('',(0.,0.,1.));
#8289=DIRECTION('center_axis',(1.,0.,0.));
#8290=DIRECTION('ref_axis',(0.,1.,0.));
#8291=DIRECTION('',(0.,1.,0.));
#8292=DIRECTION('',(0.,0.,1.));
#8293=DIRECTION('center_axis',(0.,-1.,0.));
#8294=DIRECTION('ref_axis',(1.,0.,0.));
#8295=DIRECTION('',(1.,0.,0.));
#8296=DIRECTION('',(0.,0.,1.));
#8297=DIRECTION('center_axis',(-1.,0.,0.));
#8298=DIRECTION('ref_axis',(0.,-1.,0.));
#8299=DIRECTION('',(0.,-1.,0.));
#8300=DIRECTION('',(0.,-1.,0.));
#8301=DIRECTION('center_axis',(0.,0.,1.));
#8302=DIRECTION('ref_axis',(1.,0.,0.));
#8303=DIRECTION('center_axis',(0.,0.,1.));
#8304=DIRECTION('ref_axis',(1.,0.,0.));
#8305=DIRECTION('axis',(0.,0.,1.));
#8306=DIRECTION('refdir',(1.,0.,0.));
#8307=DIRECTION('center_axis',(0.866025403784439,0.,-0.5));
#8308=DIRECTION('ref_axis',(0.5,0.,0.866025403784439));
#8309=DIRECTION('',(-0.5,0.,-0.866025403784439));
#8310=DIRECTION('',(0.,-1.,0.));
#8311=DIRECTION('',(0.5,0.,0.866025403784439));
#8312=DIRECTION('',(0.,-1.,0.));
#8313=DIRECTION('center_axis',(1.92296268638356E-16,0.,-1.));
#8314=DIRECTION('ref_axis',(1.,0.,1.92296268638356E-16));
#8315=DIRECTION('',(-1.,0.,-1.92296268638356E-16));
#8316=DIRECTION('',(0.,-1.,0.));
#8317=DIRECTION('',(1.,0.,1.92296268638356E-16));
#8318=DIRECTION('center_axis',(-0.866025403784439,0.,-0.5));
#8319=DIRECTION('ref_axis',(0.5,0.,-0.866025403784439));
#8320=DIRECTION('',(-0.5,0.,0.866025403784438));
#8321=DIRECTION('',(0.,-1.,0.));
#8322=DIRECTION('',(0.5,0.,-0.866025403784438));
#8323=DIRECTION('center_axis',(-0.866025403784439,0.,0.5));
#8324=DIRECTION('ref_axis',(-0.5,0.,-0.866025403784439));
#8325=DIRECTION('',(0.5,0.,0.866025403784439));
#8326=DIRECTION('',(0.,-1.,0.));
#8327=DIRECTION('',(-0.5,0.,-0.866025403784439));
#8328=DIRECTION('center_axis',(-1.92296268638356E-16,0.,1.));
#8329=DIRECTION('ref_axis',(-1.,0.,-1.92296268638356E-16));
#8330=DIRECTION('',(1.,0.,1.92296268638356E-16));
#8331=DIRECTION('',(0.,-1.,0.));
#8332=DIRECTION('',(-1.,0.,-1.92296268638356E-16));
#8333=DIRECTION('center_axis',(0.866025403784439,0.,0.5));
#8334=DIRECTION('ref_axis',(-0.5,0.,0.866025403784439));
#8335=DIRECTION('',(0.5,0.,-0.866025403784439));
#8336=DIRECTION('',(-0.5,0.,0.866025403784439));
#8337=DIRECTION('center_axis',(0.,1.,0.));
#8338=DIRECTION('ref_axis',(1.,0.,0.));
#8339=DIRECTION('center_axis',(0.,-1.,0.));
#8340=DIRECTION('ref_axis',(0.,0.,-1.));
#8341=DIRECTION('center_axis',(0.,1.,0.));
#8342=DIRECTION('ref_axis',(1.,0.,0.));
#8343=DIRECTION('center_axis',(0.,1.,0.));
#8344=DIRECTION('ref_axis',(1.,0.,0.));
#8345=DIRECTION('center_axis',(0.,1.,0.));
#8346=DIRECTION('ref_axis',(0.,0.,1.));
#8347=DIRECTION('center_axis',(0.,-1.,0.));
#8348=DIRECTION('ref_axis',(1.,0.,0.));
#8349=DIRECTION('center_axis',(0.,-1.,0.));
#8350=DIRECTION('ref_axis',(1.,0.,0.));
#8351=DIRECTION('center_axis',(0.,-1.,0.));
#8352=DIRECTION('ref_axis',(1.,0.,0.));
#8353=DIRECTION('',(0.707106781186548,0.707106781186547,8.65956056235494E-17));
#8354=DIRECTION('center_axis',(0.,-1.,0.));
#8355=DIRECTION('ref_axis',(1.,0.,0.));
#8356=DIRECTION('center_axis',(0.,-1.,0.));
#8357=DIRECTION('ref_axis',(1.,0.,0.));
#8358=DIRECTION('',(0.,1.,0.));
#8359=DIRECTION('center_axis',(0.,1.,0.));
#8360=DIRECTION('ref_axis',(1.,0.,0.));
#8361=DIRECTION('center_axis',(0.,-1.,0.));
#8362=DIRECTION('ref_axis',(1.,0.,0.));
#8363=DIRECTION('',(-0.707106781186547,0.707106781186548,-8.65956056235493E-17));
#8364=DIRECTION('center_axis',(0.,-1.,0.));
#8365=DIRECTION('ref_axis',(0.,0.,-1.));
#8366=DIRECTION('center_axis',(0.,-1.,0.));
#8367=DIRECTION('ref_axis',(1.,0.,0.));
#8368=DIRECTION('center_axis',(0.,1.,0.));
#8369=DIRECTION('ref_axis',(1.,0.,0.));
#8370=DIRECTION('center_axis',(0.,1.,0.));
#8371=DIRECTION('ref_axis',(1.,0.,0.));
#8372=DIRECTION('',(-0.447213595499958,0.894427190999916,-5.47678698264203E-17));
#8373=DIRECTION('center_axis',(0.,-1.,0.));
#8374=DIRECTION('ref_axis',(1.,0.,0.));
#8375=DIRECTION('',(0.,1.,0.));
#8376=DIRECTION('axis',(0.,0.,1.));
#8377=DIRECTION('refdir',(1.,0.,0.));
#8378=DIRECTION('center_axis',(0.,1.,0.));
#8379=DIRECTION('ref_axis',(1.,0.,0.));
#8380=DIRECTION('center_axis',(0.,1.,0.));
#8381=DIRECTION('ref_axis',(1.,0.,0.));
#8382=DIRECTION('',(0.,1.,0.));
#8383=DIRECTION('center_axis',(0.,-1.,0.));
#8384=DIRECTION('ref_axis',(1.,0.,0.));
#8385=DIRECTION('center_axis',(0.,1.,0.));
#8386=DIRECTION('ref_axis',(1.,0.,0.));
#8387=DIRECTION('center_axis',(0.,1.,0.));
#8388=DIRECTION('ref_axis',(1.,0.,0.));
#8389=DIRECTION('center_axis',(0.,1.,0.));
#8390=DIRECTION('ref_axis',(1.,0.,0.));
#8391=DIRECTION('center_axis',(0.,1.,0.));
#8392=DIRECTION('ref_axis',(1.,0.,0.));
#8393=DIRECTION('center_axis',(0.,1.,0.));
#8394=DIRECTION('ref_axis',(1.,0.,0.));
#8395=DIRECTION('',(0.,-1.,0.));
#8396=DIRECTION('center_axis',(0.,1.,0.));
#8397=DIRECTION('ref_axis',(1.,0.,0.));
#8398=DIRECTION('center_axis',(0.,1.,0.));
#8399=DIRECTION('ref_axis',(1.,0.,0.));
#8400=DIRECTION('center_axis',(0.,1.,0.));
#8401=DIRECTION('ref_axis',(1.,0.,0.));
#8402=DIRECTION('center_axis',(0.,1.,0.));
#8403=DIRECTION('ref_axis',(1.,0.,0.));
#8404=DIRECTION('',(0.,-1.,0.));
#8405=DIRECTION('center_axis',(0.,1.,0.));
#8406=DIRECTION('ref_axis',(1.,0.,0.));
#8407=DIRECTION('axis',(0.,0.,1.));
#8408=DIRECTION('refdir',(1.,0.,0.));
#8409=DIRECTION('center_axis',(0.,1.,0.));
#8410=DIRECTION('ref_axis',(1.,0.,0.));
#8411=DIRECTION('center_axis',(0.,-1.,0.));
#8412=DIRECTION('ref_axis',(1.,0.,0.));
#8413=DIRECTION('',(0.,-1.,0.));
#8414=DIRECTION('center_axis',(0.,-1.,0.));
#8415=DIRECTION('ref_axis',(1.,0.,0.));
#8416=DIRECTION('center_axis',(0.,1.,0.));
#8417=DIRECTION('ref_axis',(1.,0.,0.));
#8418=DIRECTION('center_axis',(0.,1.,0.));
#8419=DIRECTION('ref_axis',(1.,0.,0.));
#8420=DIRECTION('',(0.,-1.,0.));
#8421=DIRECTION('center_axis',(0.,1.,0.));
#8422=DIRECTION('ref_axis',(1.,0.,0.));
#8423=DIRECTION('center_axis',(0.,1.,0.));
#8424=DIRECTION('ref_axis',(1.,0.,0.));
#8425=DIRECTION('center_axis',(0.,1.,0.));
#8426=DIRECTION('ref_axis',(1.,0.,0.));
#8427=DIRECTION('axis',(0.,0.,1.));
#8428=DIRECTION('refdir',(1.,0.,0.));
#8429=DIRECTION('center_axis',(0.,1.,0.));
#8430=DIRECTION('ref_axis',(1.,0.,0.));
#8431=DIRECTION('center_axis',(0.,-1.,0.));
#8432=DIRECTION('ref_axis',(1.,0.,0.));
#8433=DIRECTION('',(0.,-1.,0.));
#8434=DIRECTION('center_axis',(0.,-1.,0.));
#8435=DIRECTION('ref_axis',(1.,0.,0.));
#8436=DIRECTION('center_axis',(0.,1.,0.));
#8437=DIRECTION('ref_axis',(1.,0.,0.));
#8438=DIRECTION('center_axis',(0.,1.,0.));
#8439=DIRECTION('ref_axis',(1.,0.,0.));
#8440=DIRECTION('',(0.,-1.,0.));
#8441=DIRECTION('center_axis',(0.,1.,0.));
#8442=DIRECTION('ref_axis',(1.,0.,0.));
#8443=DIRECTION('center_axis',(0.,1.,0.));
#8444=DIRECTION('ref_axis',(1.,0.,0.));
#8445=DIRECTION('center_axis',(0.,1.,0.));
#8446=DIRECTION('ref_axis',(1.,0.,0.));
#8447=DIRECTION('axis',(0.,0.,1.));
#8448=DIRECTION('refdir',(1.,0.,0.));
#8449=DIRECTION('center_axis',(0.,1.,0.));
#8450=DIRECTION('ref_axis',(1.,0.,0.));
#8451=DIRECTION('center_axis',(0.,1.,0.));
#8452=DIRECTION('ref_axis',(1.,0.,0.));
#8453=DIRECTION('',(0.,1.,0.));
#8454=DIRECTION('center_axis',(0.,-1.,0.));
#8455=DIRECTION('ref_axis',(1.,0.,0.));
#8456=DIRECTION('center_axis',(0.,1.,0.));
#8457=DIRECTION('ref_axis',(1.,0.,0.));
#8458=DIRECTION('center_axis',(0.,1.,0.));
#8459=DIRECTION('ref_axis',(1.,0.,0.));
#8460=DIRECTION('center_axis',(0.,1.,0.));
#8461=DIRECTION('ref_axis',(1.,0.,0.));
#8462=DIRECTION('center_axis',(0.,1.,0.));
#8463=DIRECTION('ref_axis',(1.,0.,0.));
#8464=DIRECTION('center_axis',(0.,1.,0.));
#8465=DIRECTION('ref_axis',(1.,0.,0.));
#8466=DIRECTION('',(0.,-1.,0.));
#8467=DIRECTION('center_axis',(0.,1.,0.));
#8468=DIRECTION('ref_axis',(1.,0.,0.));
#8469=DIRECTION('center_axis',(0.,1.,0.));
#8470=DIRECTION('ref_axis',(1.,0.,0.));
#8471=DIRECTION('center_axis',(0.,1.,0.));
#8472=DIRECTION('ref_axis',(1.,0.,0.));
#8473=DIRECTION('center_axis',(0.,1.,0.));
#8474=DIRECTION('ref_axis',(1.,0.,0.));
#8475=DIRECTION('',(0.,-1.,0.));
#8476=DIRECTION('center_axis',(0.,1.,0.));
#8477=DIRECTION('ref_axis',(1.,0.,0.));
#8478=DIRECTION('axis',(0.,0.,1.));
#8479=DIRECTION('refdir',(1.,0.,0.));
#8480=DIRECTION('center_axis',(0.,1.,0.));
#8481=DIRECTION('ref_axis',(1.,0.,0.));
#8482=DIRECTION('center_axis',(0.,-1.,0.));
#8483=DIRECTION('ref_axis',(1.,0.,0.));
#8484=DIRECTION('',(0.,-1.,0.));
#8485=DIRECTION('center_axis',(0.,-1.,0.));
#8486=DIRECTION('ref_axis',(1.,0.,0.));
#8487=DIRECTION('center_axis',(0.,1.,0.));
#8488=DIRECTION('ref_axis',(1.,0.,0.));
#8489=DIRECTION('center_axis',(0.,1.,0.));
#8490=DIRECTION('ref_axis',(1.,0.,0.));
#8491=DIRECTION('',(0.,-1.,0.));
#8492=DIRECTION('center_axis',(0.,1.,0.));
#8493=DIRECTION('ref_axis',(1.,0.,0.));
#8494=DIRECTION('center_axis',(0.,1.,0.));
#8495=DIRECTION('ref_axis',(1.,0.,0.));
#8496=DIRECTION('center_axis',(0.,1.,0.));
#8497=DIRECTION('ref_axis',(1.,0.,0.));
#8498=DIRECTION('axis',(0.,0.,1.));
#8499=DIRECTION('refdir',(1.,0.,0.));
#8500=DIRECTION('center_axis',(0.,1.,0.));
#8501=DIRECTION('ref_axis',(1.,0.,0.));
#8502=DIRECTION('center_axis',(0.,-1.,0.));
#8503=DIRECTION('ref_axis',(1.,0.,0.));
#8504=DIRECTION('',(0.,-1.,0.));
#8505=DIRECTION('center_axis',(0.,-1.,0.));
#8506=DIRECTION('ref_axis',(1.,0.,0.));
#8507=DIRECTION('center_axis',(0.,1.,0.));
#8508=DIRECTION('ref_axis',(1.,0.,0.));
#8509=DIRECTION('center_axis',(0.,1.,0.));
#8510=DIRECTION('ref_axis',(1.,0.,0.));
#8511=DIRECTION('',(0.,-1.,0.));
#8512=DIRECTION('center_axis',(0.,1.,0.));
#8513=DIRECTION('ref_axis',(1.,0.,0.));
#8514=DIRECTION('center_axis',(0.,1.,0.));
#8515=DIRECTION('ref_axis',(1.,0.,0.));
#8516=DIRECTION('center_axis',(0.,1.,0.));
#8517=DIRECTION('ref_axis',(1.,0.,0.));
#8518=DIRECTION('axis',(0.,0.,1.));
#8519=DIRECTION('refdir',(1.,0.,0.));
#8520=DIRECTION('center_axis',(0.866025403784439,0.,-0.5));
#8521=DIRECTION('ref_axis',(0.5,0.,0.866025403784439));
#8522=DIRECTION('',(-0.5,0.,-0.866025403784439));
#8523=DIRECTION('',(0.,-1.,0.));
#8524=DIRECTION('',(0.5,0.,0.866025403784439));
#8525=DIRECTION('',(0.,-1.,0.));
#8526=DIRECTION('center_axis',(1.60246890531964E-16,0.,-1.));
#8527=DIRECTION('ref_axis',(1.,0.,1.60246890531964E-16));
#8528=DIRECTION('',(-1.,0.,-1.60246890531964E-16));
#8529=DIRECTION('',(0.,-1.,0.));
#8530=DIRECTION('',(1.,0.,1.60246890531964E-16));
#8531=DIRECTION('center_axis',(-0.866025403784439,0.,-0.5));
#8532=DIRECTION('ref_axis',(0.5,0.,-0.866025403784439));
#8533=DIRECTION('',(-0.5,0.,0.866025403784439));
#8534=DIRECTION('',(0.,-1.,0.));
#8535=DIRECTION('',(0.5,0.,-0.866025403784439));
#8536=DIRECTION('center_axis',(-0.866025403784439,0.,0.5));
#8537=DIRECTION('ref_axis',(-0.5,0.,-0.866025403784439));
#8538=DIRECTION('',(0.5,0.,0.866025403784439));
#8539=DIRECTION('',(0.,-1.,0.));
#8540=DIRECTION('',(-0.5,0.,-0.866025403784439));
#8541=DIRECTION('center_axis',(-1.60246890531964E-16,0.,1.));
#8542=DIRECTION('ref_axis',(-1.,0.,-1.60246890531964E-16));
#8543=DIRECTION('',(1.,0.,1.60246890531964E-16));
#8544=DIRECTION('',(0.,-1.,0.));
#8545=DIRECTION('',(-1.,0.,-1.60246890531964E-16));
#8546=DIRECTION('center_axis',(0.866025403784439,0.,0.5));
#8547=DIRECTION('ref_axis',(-0.5,0.,0.866025403784439));
#8548=DIRECTION('',(0.5,0.,-0.866025403784439));
#8549=DIRECTION('',(-0.5,0.,0.866025403784439));
#8550=DIRECTION('center_axis',(0.,1.,0.));
#8551=DIRECTION('ref_axis',(1.,0.,0.));
#8552=DIRECTION('center_axis',(0.,-1.,0.));
#8553=DIRECTION('ref_axis',(0.,0.,-1.));
#8554=DIRECTION('center_axis',(0.,1.,0.));
#8555=DIRECTION('ref_axis',(1.,0.,0.));
#8556=DIRECTION('center_axis',(0.,1.,0.));
#8557=DIRECTION('ref_axis',(1.,0.,0.));
#8558=DIRECTION('center_axis',(0.,1.,0.));
#8559=DIRECTION('ref_axis',(0.,0.,1.));
#8560=DIRECTION('center_axis',(0.,-1.,0.));
#8561=DIRECTION('ref_axis',(1.,0.,0.));
#8562=DIRECTION('center_axis',(0.,-1.,0.));
#8563=DIRECTION('ref_axis',(1.,0.,0.));
#8564=DIRECTION('center_axis',(0.,-1.,0.));
#8565=DIRECTION('ref_axis',(1.,0.,0.));
#8566=DIRECTION('',(0.707106781186547,0.707106781186548,8.65956056235493E-17));
#8567=DIRECTION('center_axis',(0.,-1.,0.));
#8568=DIRECTION('ref_axis',(1.,0.,0.));
#8569=DIRECTION('center_axis',(0.,-1.,0.));
#8570=DIRECTION('ref_axis',(1.,0.,0.));
#8571=DIRECTION('',(0.,1.,0.));
#8572=DIRECTION('center_axis',(0.,1.,0.));
#8573=DIRECTION('ref_axis',(1.,0.,0.));
#8574=DIRECTION('center_axis',(0.,-1.,0.));
#8575=DIRECTION('ref_axis',(1.,0.,0.));
#8576=DIRECTION('',(-0.707106781186547,0.707106781186548,-8.65956056235493E-17));
#8577=DIRECTION('center_axis',(0.,-1.,0.));
#8578=DIRECTION('ref_axis',(0.,0.,-1.));
#8579=DIRECTION('center_axis',(0.,-1.,0.));
#8580=DIRECTION('ref_axis',(1.,0.,0.));
#8581=DIRECTION('center_axis',(0.,1.,0.));
#8582=DIRECTION('ref_axis',(1.,0.,0.));
#8583=DIRECTION('center_axis',(0.,1.,0.));
#8584=DIRECTION('ref_axis',(1.,0.,0.));
#8585=DIRECTION('',(-0.447213595499958,0.894427190999916,-5.47678698264203E-17));
#8586=DIRECTION('center_axis',(0.,-1.,0.));
#8587=DIRECTION('ref_axis',(1.,0.,0.));
#8588=DIRECTION('',(0.,1.,0.));
#8589=DIRECTION('axis',(0.,0.,1.));
#8590=DIRECTION('refdir',(1.,0.,0.));
#8591=DIRECTION('center_axis',(0.,0.,1.));
#8592=DIRECTION('ref_axis',(1.,0.,0.));
#8593=DIRECTION('center_axis',(0.,0.,1.));
#8594=DIRECTION('ref_axis',(1.,0.,0.));
#8595=DIRECTION('',(0.,0.,-1.));
#8596=DIRECTION('center_axis',(0.,0.,-1.));
#8597=DIRECTION('ref_axis',(1.,0.,0.));
#8598=DIRECTION('center_axis',(0.,0.,1.));
#8599=DIRECTION('ref_axis',(1.,0.,0.));
#8600=DIRECTION('center_axis',(0.,0.,1.));
#8601=DIRECTION('ref_axis',(1.,0.,0.));
#8602=DIRECTION('center_axis',(0.,0.,1.));
#8603=DIRECTION('ref_axis',(1.,0.,0.));
#8604=DIRECTION('',(0.,0.,1.));
#8605=DIRECTION('center_axis',(0.,0.,-1.));
#8606=DIRECTION('ref_axis',(1.,0.,0.));
#8607=DIRECTION('center_axis',(0.,0.,1.));
#8608=DIRECTION('ref_axis',(1.,0.,0.));
#8609=DIRECTION('center_axis',(0.,0.,1.));
#8610=DIRECTION('ref_axis',(1.,0.,0.));
#8611=DIRECTION('',(0.,0.,1.));
#8612=DIRECTION('center_axis',(0.,0.,-1.));
#8613=DIRECTION('ref_axis',(1.,0.,0.));
#8614=DIRECTION('center_axis',(0.,1.,0.));
#8615=DIRECTION('ref_axis',(-1.,0.,0.));
#8616=DIRECTION('',(-1.,0.,0.));
#8617=DIRECTION('',(0.,0.,1.));
#8618=DIRECTION('',(-1.,0.,0.));
#8619=DIRECTION('',(0.,0.,1.));
#8620=DIRECTION('center_axis',(1.,0.,0.));
#8621=DIRECTION('ref_axis',(0.,1.,0.));
#8622=DIRECTION('',(0.,1.,0.));
#8623=DIRECTION('',(0.,1.,0.));
#8624=DIRECTION('',(0.,0.,1.));
#8625=DIRECTION('center_axis',(0.,-1.,0.));
#8626=DIRECTION('ref_axis',(1.,0.,0.));
#8627=DIRECTION('',(1.,0.,0.));
#8628=DIRECTION('',(1.,0.,0.));
#8629=DIRECTION('',(0.,0.,1.));
#8630=DIRECTION('center_axis',(-1.,0.,0.));
#8631=DIRECTION('ref_axis',(0.,-1.,0.));
#8632=DIRECTION('',(0.,-1.,0.));
#8633=DIRECTION('',(0.,-1.,0.));
#8634=DIRECTION('center_axis',(0.,0.,1.));
#8635=DIRECTION('ref_axis',(1.,0.,0.));
#8636=DIRECTION('center_axis',(0.,0.,1.));
#8637=DIRECTION('ref_axis',(1.,0.,0.));
#8638=DIRECTION('axis',(0.,0.,1.));
#8639=DIRECTION('refdir',(1.,0.,0.));
#8640=DIRECTION('center_axis',(0.866025403784439,0.,-0.5));
#8641=DIRECTION('ref_axis',(0.5,0.,0.866025403784439));
#8642=DIRECTION('',(-0.5,0.,-0.866025403784439));
#8643=DIRECTION('',(0.,-1.,0.));
#8644=DIRECTION('',(0.5,0.,0.866025403784439));
#8645=DIRECTION('',(0.,-1.,0.));
#8646=DIRECTION('center_axis',(1.20185167898973E-16,0.,-1.));
#8647=DIRECTION('ref_axis',(1.,0.,1.20185167898973E-16));
#8648=DIRECTION('',(-1.,0.,-1.20185167898973E-16));
#8649=DIRECTION('',(0.,-1.,0.));
#8650=DIRECTION('',(1.,0.,1.20185167898973E-16));
#8651=DIRECTION('center_axis',(-0.866025403784439,0.,-0.5));
#8652=DIRECTION('ref_axis',(0.5,0.,-0.866025403784439));
#8653=DIRECTION('',(-0.5,0.,0.866025403784439));
#8654=DIRECTION('',(0.,-1.,0.));
#8655=DIRECTION('',(0.5,0.,-0.866025403784439));
#8656=DIRECTION('center_axis',(-0.866025403784439,0.,0.5));
#8657=DIRECTION('ref_axis',(-0.5,0.,-0.866025403784439));
#8658=DIRECTION('',(0.5,0.,0.866025403784439));
#8659=DIRECTION('',(0.,-1.,0.));
#8660=DIRECTION('',(-0.5,0.,-0.866025403784439));
#8661=DIRECTION('center_axis',(-2.40370335797945E-16,0.,1.));
#8662=DIRECTION('ref_axis',(-1.,0.,-2.40370335797945E-16));
#8663=DIRECTION('',(1.,0.,2.40370335797945E-16));
#8664=DIRECTION('',(0.,-1.,0.));
#8665=DIRECTION('',(-1.,0.,-2.40370335797945E-16));
#8666=DIRECTION('center_axis',(0.866025403784439,0.,0.5));
#8667=DIRECTION('ref_axis',(-0.5,0.,0.866025403784439));
#8668=DIRECTION('',(0.5,0.,-0.866025403784439));
#8669=DIRECTION('',(-0.5,0.,0.866025403784439));
#8670=DIRECTION('center_axis',(0.,1.,0.));
#8671=DIRECTION('ref_axis',(1.,0.,0.));
#8672=DIRECTION('center_axis',(0.,-1.,0.));
#8673=DIRECTION('ref_axis',(0.,0.,-1.));
#8674=DIRECTION('center_axis',(0.,1.,0.));
#8675=DIRECTION('ref_axis',(1.,0.,0.));
#8676=DIRECTION('center_axis',(0.,1.,0.));
#8677=DIRECTION('ref_axis',(1.,0.,0.));
#8678=DIRECTION('center_axis',(0.,1.,0.));
#8679=DIRECTION('ref_axis',(0.,0.,1.));
#8680=DIRECTION('center_axis',(0.,-1.,0.));
#8681=DIRECTION('ref_axis',(1.,0.,0.));
#8682=DIRECTION('center_axis',(0.,-1.,0.));
#8683=DIRECTION('ref_axis',(1.,0.,0.));
#8684=DIRECTION('center_axis',(0.,-1.,0.));
#8685=DIRECTION('ref_axis',(1.,0.,0.));
#8686=DIRECTION('',(0.707106781186548,0.707106781186547,8.65956056235493E-17));
#8687=DIRECTION('center_axis',(0.,-1.,0.));
#8688=DIRECTION('ref_axis',(1.,0.,0.));
#8689=DIRECTION('center_axis',(0.,-1.,0.));
#8690=DIRECTION('ref_axis',(1.,0.,0.));
#8691=DIRECTION('',(0.,1.,0.));
#8692=DIRECTION('center_axis',(0.,1.,0.));
#8693=DIRECTION('ref_axis',(1.,0.,0.));
#8694=DIRECTION('center_axis',(0.,-1.,0.));
#8695=DIRECTION('ref_axis',(1.,0.,0.));
#8696=DIRECTION('',(-0.707106781186547,0.707106781186548,-8.65956056235493E-17));
#8697=DIRECTION('center_axis',(0.,-1.,0.));
#8698=DIRECTION('ref_axis',(0.,0.,-1.));
#8699=DIRECTION('center_axis',(0.,-1.,0.));
#8700=DIRECTION('ref_axis',(1.,0.,0.));
#8701=DIRECTION('center_axis',(0.,1.,0.));
#8702=DIRECTION('ref_axis',(1.,0.,0.));
#8703=DIRECTION('center_axis',(0.,1.,0.));
#8704=DIRECTION('ref_axis',(1.,0.,0.));
#8705=DIRECTION('',(-0.447213595499958,0.894427190999916,-5.47678698264203E-17));
#8706=DIRECTION('center_axis',(0.,-1.,0.));
#8707=DIRECTION('ref_axis',(1.,0.,0.));
#8708=DIRECTION('',(0.,1.,0.));
#8709=DIRECTION('axis',(0.,0.,1.));
#8710=DIRECTION('refdir',(1.,0.,0.));
#8711=DIRECTION('center_axis',(0.,1.,0.));
#8712=DIRECTION('ref_axis',(1.,0.,0.));
#8713=DIRECTION('',(0.,0.,1.));
#8714=DIRECTION('center_axis',(0.,1.,0.));
#8715=DIRECTION('ref_axis',(1.,0.,0.));
#8716=DIRECTION('center_axis',(0.,1.,0.));
#8717=DIRECTION('ref_axis',(1.,0.,0.));
#8718=DIRECTION('center_axis',(0.,1.,0.));
#8719=DIRECTION('ref_axis',(1.,0.,0.));
#8720=DIRECTION('center_axis',(0.,1.,0.));
#8721=DIRECTION('ref_axis',(1.,0.,0.));
#8722=DIRECTION('',(0.,1.,0.));
#8723=DIRECTION('center_axis',(0.,-1.,0.));
#8724=DIRECTION('ref_axis',(1.,0.,0.));
#8725=DIRECTION('center_axis',(0.,1.,0.));
#8726=DIRECTION('ref_axis',(1.,0.,0.));
#8727=DIRECTION('',(0.,0.,-1.));
#8728=DIRECTION('center_axis',(0.,1.,0.));
#8729=DIRECTION('ref_axis',(1.,0.,0.));
#8730=DIRECTION('',(0.,0.,1.));
#8731=DIRECTION('center_axis',(0.,1.,0.));
#8732=DIRECTION('ref_axis',(1.,0.,0.));
#8733=DIRECTION('center_axis',(0.,1.,0.));
#8734=DIRECTION('ref_axis',(1.,0.,0.));
#8735=DIRECTION('center_axis',(0.,1.,0.));
#8736=DIRECTION('ref_axis',(1.,0.,0.));
#8737=DIRECTION('center_axis',(0.,1.,0.));
#8738=DIRECTION('ref_axis',(1.,0.,0.));
#8739=DIRECTION('',(0.,1.,0.));
#8740=DIRECTION('center_axis',(0.,-1.,0.));
#8741=DIRECTION('ref_axis',(1.,0.,0.));
#8742=DIRECTION('center_axis',(0.,1.,0.));
#8743=DIRECTION('ref_axis',(1.,0.,0.));
#8744=DIRECTION('',(0.,0.,-1.));
#8745=DIRECTION('center_axis',(0.,0.,1.));
#8746=DIRECTION('ref_axis',(1.,0.,0.));
#8747=DIRECTION('center_axis',(0.,0.,1.));
#8748=DIRECTION('ref_axis',(1.,0.,0.));
#8749=DIRECTION('',(0.,0.,1.));
#8750=DIRECTION('center_axis',(0.,0.,-1.));
#8751=DIRECTION('ref_axis',(1.,0.,0.));
#8752=DIRECTION('center_axis',(0.,0.,1.));
#8753=DIRECTION('ref_axis',(1.,0.,0.));
#8754=DIRECTION('center_axis',(0.,0.,1.));
#8755=DIRECTION('ref_axis',(1.,0.,0.));
#8756=DIRECTION('',(0.,0.,1.));
#8757=DIRECTION('center_axis',(0.,0.,-1.));
#8758=DIRECTION('ref_axis',(1.,0.,0.));
#8759=DIRECTION('center_axis',(0.,1.,0.));
#8760=DIRECTION('ref_axis',(-1.,0.,0.));
#8761=DIRECTION('',(-1.,0.,0.));
#8762=DIRECTION('',(0.,0.,1.));
#8763=DIRECTION('',(-1.,0.,0.));
#8764=DIRECTION('',(0.,0.,1.));
#8765=DIRECTION('center_axis',(1.,0.,0.));
#8766=DIRECTION('ref_axis',(0.,1.,0.));
#8767=DIRECTION('',(0.,1.,0.));
#8768=DIRECTION('',(0.,1.,0.));
#8769=DIRECTION('',(0.,0.,1.));
#8770=DIRECTION('center_axis',(0.,-1.,0.));
#8771=DIRECTION('ref_axis',(1.,0.,0.));
#8772=DIRECTION('',(1.,0.,0.));
#8773=DIRECTION('',(1.,0.,0.));
#8774=DIRECTION('',(0.,0.,1.));
#8775=DIRECTION('center_axis',(-1.,0.,0.));
#8776=DIRECTION('ref_axis',(0.,-1.,0.));
#8777=DIRECTION('',(0.,-1.,0.));
#8778=DIRECTION('',(0.,-1.,0.));
#8779=DIRECTION('center_axis',(0.,0.,1.));
#8780=DIRECTION('ref_axis',(1.,0.,0.));
#8781=DIRECTION('center_axis',(0.,0.,1.));
#8782=DIRECTION('ref_axis',(1.,0.,0.));
#8783=DIRECTION('axis',(0.,0.,1.));
#8784=DIRECTION('refdir',(1.,0.,0.));
#8785=DIRECTION('center_axis',(0.866025403784439,0.,-0.5));
#8786=DIRECTION('ref_axis',(0.5,0.,0.866025403784439));
#8787=DIRECTION('',(0.5,0.,0.866025403784439));
#8788=DIRECTION('',(0.,-1.,0.));
#8789=DIRECTION('',(0.5,0.,0.866025403784439));
#8790=DIRECTION('',(0.,-1.,0.));
#8791=DIRECTION('center_axis',(1.92296268638356E-16,0.,-1.));
#8792=DIRECTION('ref_axis',(1.,0.,1.92296268638356E-16));
#8793=DIRECTION('',(1.,0.,1.92296268638356E-16));
#8794=DIRECTION('',(0.,-1.,0.));
#8795=DIRECTION('',(1.,0.,1.92296268638356E-16));
#8796=DIRECTION('center_axis',(-0.866025403784439,0.,-0.5));
#8797=DIRECTION('ref_axis',(0.5,0.,-0.866025403784439));
#8798=DIRECTION('',(0.5,0.,-0.866025403784439));
#8799=DIRECTION('',(0.,-1.,0.));
#8800=DIRECTION('',(0.5,0.,-0.866025403784438));
#8801=DIRECTION('center_axis',(-0.866025403784439,0.,0.5));
#8802=DIRECTION('ref_axis',(-0.5,0.,-0.866025403784439));
#8803=DIRECTION('',(-0.5,0.,-0.866025403784439));
#8804=DIRECTION('',(0.,-1.,0.));
#8805=DIRECTION('',(-0.5,0.,-0.866025403784439));
#8806=DIRECTION('center_axis',(-1.92296268638356E-16,0.,1.));
#8807=DIRECTION('ref_axis',(-1.,0.,-1.92296268638356E-16));
#8808=DIRECTION('',(-1.,0.,-1.92296268638356E-16));
#8809=DIRECTION('',(0.,-1.,0.));
#8810=DIRECTION('',(-1.,0.,-1.92296268638356E-16));
#8811=DIRECTION('center_axis',(0.866025403784439,0.,0.5));
#8812=DIRECTION('ref_axis',(-0.5,0.,0.866025403784439));
#8813=DIRECTION('',(-0.5,0.,0.866025403784439));
#8814=DIRECTION('',(-0.5,0.,0.866025403784439));
#8815=DIRECTION('center_axis',(0.,-1.,0.));
#8816=DIRECTION('ref_axis',(0.,0.,-1.));
#8817=DIRECTION('center_axis',(0.,1.,0.));
#8818=DIRECTION('ref_axis',(0.,0.,1.));
#8819=DIRECTION('center_axis',(0.,-1.,0.));
#8820=DIRECTION('ref_axis',(1.,0.,0.));
#8821=DIRECTION('center_axis',(0.,-1.,0.));
#8822=DIRECTION('ref_axis',(1.,0.,0.));
#8823=DIRECTION('center_axis',(0.,-1.,0.));
#8824=DIRECTION('ref_axis',(1.,0.,0.));
#8825=DIRECTION('',(0.707106781186547,0.707106781186548,8.65956056235493E-17));
#8826=DIRECTION('center_axis',(0.,-1.,0.));
#8827=DIRECTION('ref_axis',(1.,0.,0.));
#8828=DIRECTION('center_axis',(0.,1.,0.));
#8829=DIRECTION('ref_axis',(1.,0.,0.));
#8830=DIRECTION('',(0.,1.,0.));
#8831=DIRECTION('center_axis',(0.,1.,0.));
#8832=DIRECTION('ref_axis',(1.,0.,0.));
#8833=DIRECTION('center_axis',(0.,-1.,0.));
#8834=DIRECTION('ref_axis',(1.,0.,0.));
#8835=DIRECTION('',(-0.707106781186547,0.707106781186548,-8.65956056235493E-17));
#8836=DIRECTION('center_axis',(0.,-1.,0.));
#8837=DIRECTION('ref_axis',(0.,0.,-1.));
#8838=DIRECTION('axis',(0.,0.,1.));
#8839=DIRECTION('refdir',(1.,0.,0.));
#8840=DIRECTION('center_axis',(0.,0.,1.));
#8841=DIRECTION('ref_axis',(1.,0.,0.));
#8842=DIRECTION('center_axis',(0.,0.,1.));
#8843=DIRECTION('ref_axis',(1.,0.,0.));
#8844=DIRECTION('',(0.,0.,1.));
#8845=DIRECTION('center_axis',(0.,0.,1.));
#8846=DIRECTION('ref_axis',(1.,0.,0.));
#8847=DIRECTION('center_axis',(0.,0.,1.));
#8848=DIRECTION('ref_axis',(1.,0.,0.));
#8849=DIRECTION('center_axis',(0.,0.,1.));
#8850=DIRECTION('ref_axis',(1.,0.,0.));
#8851=DIRECTION('',(0.,0.,-1.));
#8852=DIRECTION('center_axis',(0.,0.,1.));
#8853=DIRECTION('ref_axis',(1.,0.,0.));
#8854=DIRECTION('center_axis',(0.,0.,1.));
#8855=DIRECTION('ref_axis',(1.,0.,0.));
#8856=DIRECTION('center_axis',(0.,1.,0.));
#8857=DIRECTION('ref_axis',(1.,0.,0.));
#8858=DIRECTION('center_axis',(0.,1.,0.));
#8859=DIRECTION('ref_axis',(1.,0.,0.));
#8860=DIRECTION('',(0.,-1.,0.));
#8861=DIRECTION('center_axis',(0.,1.,0.));
#8862=DIRECTION('ref_axis',(1.,0.,0.));
#8863=DIRECTION('center_axis',(0.,1.,0.));
#8864=DIRECTION('ref_axis',(1.,0.,0.));
#8865=DIRECTION('center_axis',(0.,1.,0.));
#8866=DIRECTION('ref_axis',(1.,0.,0.));
#8867=DIRECTION('axis',(0.,0.,1.));
#8868=DIRECTION('refdir',(1.,0.,0.));
#8869=DIRECTION('center_axis',(0.,1.,0.));
#8870=DIRECTION('ref_axis',(1.,0.,0.));
#8871=DIRECTION('center_axis',(0.,1.,0.));
#8872=DIRECTION('ref_axis',(1.,0.,0.));
#8873=DIRECTION('',(0.,-1.,0.));
#8874=DIRECTION('center_axis',(0.,1.,0.));
#8875=DIRECTION('ref_axis',(1.,0.,0.));
#8876=DIRECTION('center_axis',(0.,1.,0.));
#8877=DIRECTION('ref_axis',(1.,0.,0.));
#8878=DIRECTION('center_axis',(0.,1.,0.));
#8879=DIRECTION('ref_axis',(1.,0.,0.));
#8880=DIRECTION('axis',(0.,0.,1.));
#8881=DIRECTION('refdir',(1.,0.,0.));
#8882=DIRECTION('center_axis',(-0.999261174631314,0.,0.0384331221012044));
#8883=DIRECTION('ref_axis',(0.0384331221012044,0.,0.999261174631314));
#8884=DIRECTION('',(-0.0384331221012044,0.,-0.999261174631314));
#8885=DIRECTION('',(0.,1.,0.));
#8886=DIRECTION('',(0.0384331221012044,0.,0.999261174631314));
#8887=DIRECTION('',(0.,1.,0.));
#8888=DIRECTION('center_axis',(0.,0.,-1.));
#8889=DIRECTION('ref_axis',(-1.,0.,0.));
#8890=DIRECTION('',(1.,0.,0.));
#8891=DIRECTION('',(-1.,0.,0.));
#8892=DIRECTION('',(0.,1.,0.));
#8893=DIRECTION('center_axis',(0.999261174631314,0.,0.0384331221012044));
#8894=DIRECTION('ref_axis',(0.0384331221012044,0.,-0.999261174631314));
#8895=DIRECTION('',(-0.0384331221012044,0.,0.999261174631314));
#8896=DIRECTION('',(0.0384331221012044,0.,-0.999261174631314));
#8897=DIRECTION('center_axis',(0.,1.,0.));
#8898=DIRECTION('ref_axis',(0.,0.,1.));
#8899=DIRECTION('center_axis',(0.,1.,0.));
#8900=DIRECTION('ref_axis',(1.,0.,0.));
#8901=DIRECTION('axis',(0.,0.,1.));
#8902=DIRECTION('refdir',(1.,0.,0.));
#8903=DIRECTION('center_axis',(0.,0.,1.));
#8904=DIRECTION('ref_axis',(1.,0.,0.));
#8905=DIRECTION('center_axis',(0.,0.,1.));
#8906=DIRECTION('ref_axis',(1.,0.,0.));
#8907=DIRECTION('',(0.,0.,-1.));
#8908=DIRECTION('center_axis',(0.,0.,1.));
#8909=DIRECTION('ref_axis',(1.,0.,0.));
#8910=DIRECTION('center_axis',(0.,0.,1.));
#8911=DIRECTION('ref_axis',(1.,0.,0.));
#8912=DIRECTION('center_axis',(0.,0.,1.));
#8913=DIRECTION('ref_axis',(1.,0.,0.));
#8914=DIRECTION('axis',(0.,0.,1.));
#8915=DIRECTION('refdir',(1.,0.,0.));
#8916=DIRECTION('center_axis',(0.,1.,0.));
#8917=DIRECTION('ref_axis',(1.,0.,0.));
#8918=DIRECTION('center_axis',(0.,-1.,0.));
#8919=DIRECTION('ref_axis',(1.,0.,0.));
#8920=DIRECTION('',(0.,-1.,0.));
#8921=DIRECTION('center_axis',(0.,-1.,0.));
#8922=DIRECTION('ref_axis',(1.,0.,0.));
#8923=DIRECTION('center_axis',(0.,1.,0.));
#8924=DIRECTION('ref_axis',(1.,0.,0.));
#8925=DIRECTION('center_axis',(0.,1.,0.));
#8926=DIRECTION('ref_axis',(1.,0.,0.));
#8927=DIRECTION('',(0.,-1.,0.));
#8928=DIRECTION('center_axis',(0.,1.,0.));
#8929=DIRECTION('ref_axis',(1.,0.,0.));
#8930=DIRECTION('center_axis',(0.,1.,0.));
#8931=DIRECTION('ref_axis',(1.,0.,0.));
#8932=DIRECTION('center_axis',(0.,1.,0.));
#8933=DIRECTION('ref_axis',(1.,0.,0.));
#8934=DIRECTION('axis',(0.,0.,1.));
#8935=DIRECTION('refdir',(1.,0.,0.));
#8936=DIRECTION('center_axis',(0.,1.,0.));
#8937=DIRECTION('ref_axis',(1.,0.,0.));
#8938=DIRECTION('center_axis',(0.,-1.,0.));
#8939=DIRECTION('ref_axis',(1.,0.,0.));
#8940=DIRECTION('',(0.,-1.,0.));
#8941=DIRECTION('center_axis',(0.,-1.,0.));
#8942=DIRECTION('ref_axis',(1.,0.,0.));
#8943=DIRECTION('center_axis',(0.,1.,0.));
#8944=DIRECTION('ref_axis',(1.,0.,0.));
#8945=DIRECTION('center_axis',(0.,1.,0.));
#8946=DIRECTION('ref_axis',(1.,0.,0.));
#8947=DIRECTION('',(0.,-1.,0.));
#8948=DIRECTION('center_axis',(0.,1.,0.));
#8949=DIRECTION('ref_axis',(1.,0.,0.));
#8950=DIRECTION('center_axis',(0.,1.,0.));
#8951=DIRECTION('ref_axis',(1.,0.,0.));
#8952=DIRECTION('center_axis',(0.,1.,0.));
#8953=DIRECTION('ref_axis',(1.,0.,0.));
#8954=DIRECTION('axis',(0.,0.,1.));
#8955=DIRECTION('refdir',(1.,0.,0.));
#8956=DIRECTION('center_axis',(0.,1.,0.));
#8957=DIRECTION('ref_axis',(1.,0.,0.));
#8958=DIRECTION('center_axis',(0.,-1.,0.));
#8959=DIRECTION('ref_axis',(1.,0.,0.));
#8960=DIRECTION('',(0.,-1.,0.));
#8961=DIRECTION('center_axis',(0.,-1.,0.));
#8962=DIRECTION('ref_axis',(1.,0.,0.));
#8963=DIRECTION('center_axis',(0.,1.,0.));
#8964=DIRECTION('ref_axis',(1.,0.,0.));
#8965=DIRECTION('center_axis',(0.,1.,0.));
#8966=DIRECTION('ref_axis',(1.,0.,0.));
#8967=DIRECTION('',(0.,-1.,0.));
#8968=DIRECTION('center_axis',(0.,1.,0.));
#8969=DIRECTION('ref_axis',(1.,0.,0.));
#8970=DIRECTION('center_axis',(0.,1.,0.));
#8971=DIRECTION('ref_axis',(1.,0.,0.));
#8972=DIRECTION('center_axis',(0.,1.,0.));
#8973=DIRECTION('ref_axis',(1.,0.,0.));
#8974=DIRECTION('',(0.,0.,1.));
#8975=DIRECTION('',(2.22044604925031E-16,1.,0.));
#8976=DIRECTION('',(0.,0.,1.));
#8977=DIRECTION('',(2.22044604925031E-16,1.,0.));
#8978=DIRECTION('',(0.,0.,1.));
#8979=DIRECTION('',(1.,0.,0.));
#8980=DIRECTION('',(0.,0.,1.));
#8981=DIRECTION('',(2.22044604925031E-16,1.,0.));
#8982=DIRECTION('',(0.,-1.,2.22044604925031E-16));
#8983=DIRECTION('',(1.,0.,0.));
#8984=DIRECTION('',(0.,-1.,2.22044604925031E-16));
#8985=DIRECTION('',(1.,0.,0.));
#8986=DIRECTION('',(0.,0.,1.));
#8987=DIRECTION('',(2.22044604925031E-16,1.,0.));
#8988=DIRECTION('',(0.,-1.,2.22044604925031E-16));
#8989=DIRECTION('',(1.,0.,0.));
#8990=DIRECTION('',(0.,-1.,2.22044604925031E-16));
#8991=DIRECTION('',(1.,0.,0.));
#8992=DIRECTION('',(0.,0.,1.));
#8993=DIRECTION('',(2.22044604925031E-16,1.,0.));
#8994=DIRECTION('',(0.,-1.,2.22044604925031E-16));
#8995=DIRECTION('',(1.,0.,0.));
#8996=DIRECTION('',(0.,-1.,2.22044604925031E-16));
#8997=DIRECTION('',(1.,0.,0.));
#8998=DIRECTION('',(0.,0.,1.));
#8999=DIRECTION('',(2.22044604925031E-16,1.,0.));
#9000=DIRECTION('',(0.,-1.,2.22044604925031E-16));
#9001=DIRECTION('',(1.,0.,0.));
#9002=DIRECTION('',(0.,-1.,2.22044604925031E-16));
#9003=DIRECTION('',(1.,0.,0.));
#9004=DIRECTION('',(0.,0.,1.));
#9005=DIRECTION('',(2.22044604925031E-16,1.,0.));
#9006=DIRECTION('',(0.,-1.,2.22044604925031E-16));
#9007=DIRECTION('',(1.,0.,0.));
#9008=DIRECTION('',(0.,-1.,2.22044604925031E-16));
#9009=DIRECTION('',(1.,0.,0.));
#9010=DIRECTION('',(0.,0.,1.));
#9011=DIRECTION('',(2.22044604925031E-16,1.,0.));
#9012=DIRECTION('',(0.,-1.,2.22044604925031E-16));
#9013=DIRECTION('',(1.,0.,0.));
#9014=DIRECTION('',(0.,-1.,2.22044604925031E-16));
#9015=DIRECTION('',(1.,0.,0.));
#9016=DIRECTION('',(0.,0.,1.));
#9017=DIRECTION('',(1.,0.,0.));
#9018=DIRECTION('',(0.,0.,1.));
#9019=DIRECTION('',(1.,0.,0.));
#9020=DIRECTION('',(0.,0.,1.));
#9021=DIRECTION('',(1.,0.,0.));
#9022=DIRECTION('',(0.,-1.,2.22044604925031E-16));
#9023=DIRECTION('',(1.,0.,0.));
#9024=DIRECTION('',(0.,-1.,2.22044604925031E-16));
#9025=DIRECTION('',(1.,0.,0.));
#9026=DIRECTION('',(0.,0.,1.));
#9027=DIRECTION('',(1.,0.,0.));
#9028=DIRECTION('',(0.,0.,1.));
#9029=DIRECTION('',(1.,0.,0.));
#9030=DIRECTION('',(0.,0.,1.));
#9031=DIRECTION('',(1.,0.,0.));
#9032=DIRECTION('',(0.,0.,1.));
#9033=DIRECTION('',(1.,0.,0.));
#9034=DIRECTION('',(0.,0.,1.));
#9035=DIRECTION('',(1.,0.,0.));
#9036=DIRECTION('',(0.,0.,1.));
#9037=DIRECTION('',(1.,0.,0.));
#9038=DIRECTION('',(0.,0.,1.));
#9039=DIRECTION('',(1.,0.,0.));
#9040=DIRECTION('',(0.,0.,1.));
#9041=DIRECTION('',(1.,0.,0.));
#9042=DIRECTION('',(0.,0.,1.));
#9043=DIRECTION('',(1.,0.,0.));
#9044=DIRECTION('',(0.,0.,1.));
#9045=DIRECTION('',(1.,0.,0.));
#9046=DIRECTION('',(0.,-1.,2.22044604925031E-16));
#9047=DIRECTION('',(1.,0.,0.));
#9048=DIRECTION('',(0.,-1.,2.22044604925031E-16));
#9049=DIRECTION('',(1.,0.,0.));
#9050=DIRECTION('',(0.,0.,1.));
#9051=DIRECTION('',(1.,0.,0.));
#9052=DIRECTION('',(0.,0.,1.));
#9053=DIRECTION('',(1.,0.,0.));
#9054=DIRECTION('',(0.,0.,1.));
#9055=DIRECTION('',(1.,0.,0.));
#9056=DIRECTION('',(0.,0.,1.));
#9057=DIRECTION('',(1.,0.,0.));
#9058=DIRECTION('',(0.,0.,1.));
#9059=DIRECTION('',(1.,0.,0.));
#9060=DIRECTION('',(0.,0.,1.));
#9061=DIRECTION('',(1.,0.,0.));
#9062=DIRECTION('',(0.,0.,1.));
#9063=DIRECTION('',(1.,0.,0.));
#9064=DIRECTION('',(0.,0.,1.));
#9065=DIRECTION('',(1.,0.,0.));
#9066=DIRECTION('',(0.,0.,1.));
#9067=DIRECTION('',(1.,0.,0.));
#9068=DIRECTION('',(0.,-1.,2.22044604925031E-16));
#9069=DIRECTION('',(1.,0.,0.));
#9070=DIRECTION('',(0.,-1.,2.22044604925031E-16));
#9071=DIRECTION('',(1.,0.,0.));
#9072=DIRECTION('',(0.,0.,1.));
#9073=DIRECTION('',(1.,0.,0.));
#9074=DIRECTION('',(0.,0.,1.));
#9075=DIRECTION('',(1.,0.,0.));
#9076=DIRECTION('',(0.,0.,1.));
#9077=DIRECTION('',(1.,0.,0.));
#9078=DIRECTION('',(0.,0.,1.));
#9079=DIRECTION('',(1.,0.,0.));
#9080=DIRECTION('',(0.,0.,1.));
#9081=DIRECTION('',(1.,0.,0.));
#9082=DIRECTION('',(0.,0.,1.));
#9083=DIRECTION('',(1.,0.,0.));
#9084=DIRECTION('',(0.,0.,1.));
#9085=DIRECTION('',(1.,0.,0.));
#9086=DIRECTION('',(0.,0.,1.));
#9087=DIRECTION('',(1.,0.,0.));
#9088=DIRECTION('',(0.,0.,1.));
#9089=DIRECTION('',(1.,0.,0.));
#9090=DIRECTION('',(0.,0.,1.));
#9091=DIRECTION('',(1.,0.,0.));
#9092=DIRECTION('axis',(0.,0.,1.));
#9093=DIRECTION('refdir',(1.,0.,0.));
#9094=DIRECTION('axis',(0.,0.,1.));
#9095=DIRECTION('refdir',(1.,0.,0.));
#9096=DIRECTION('center_axis',(0.,1.,0.));
#9097=DIRECTION('ref_axis',(1.,0.,0.));
#9098=DIRECTION('center_axis',(0.,1.,0.));
#9099=DIRECTION('ref_axis',(1.,0.,0.));
#9100=DIRECTION('',(0.,-1.,0.));
#9101=DIRECTION('center_axis',(0.,1.,0.));
#9102=DIRECTION('ref_axis',(1.,0.,0.));
#9103=DIRECTION('center_axis',(0.,1.,0.));
#9104=DIRECTION('ref_axis',(1.,0.,0.));
#9105=DIRECTION('center_axis',(0.,1.,0.));
#9106=DIRECTION('ref_axis',(1.,0.,0.));
#9107=DIRECTION('',(0.,0.,1.));
#9108=DIRECTION('',(1.,0.,0.));
#9109=DIRECTION('axis',(0.,0.,1.));
#9110=DIRECTION('refdir',(1.,0.,0.));
#9111=DIRECTION('axis',(0.,0.,1.));
#9112=DIRECTION('refdir',(1.,0.,0.));
#9113=DIRECTION('axis',(0.,0.,1.));
#9114=DIRECTION('refdir',(1.,0.,0.));
#9115=DIRECTION('center_axis',(0.,-1.,0.));
#9116=DIRECTION('ref_axis',(0.,0.,-1.));
#9117=DIRECTION('center_axis',(0.,-1.,0.));
#9118=DIRECTION('ref_axis',(1.,0.,0.));
#9119=DIRECTION('center_axis',(0.,-1.,0.));
#9120=DIRECTION('ref_axis',(1.,0.,0.));
#9121=DIRECTION('center_axis',(1.,0.,1.22464679914735E-16));
#9122=DIRECTION('ref_axis',(-1.22464679914735E-16,0.,1.));
#9123=DIRECTION('center_axis',(0.,1.,0.));
#9124=DIRECTION('ref_axis',(1.,0.,0.));
#9125=DIRECTION('center_axis',(0.,1.,0.));
#9126=DIRECTION('ref_axis',(1.,0.,0.));
#9127=DIRECTION('center_axis',(0.,-1.,0.));
#9128=DIRECTION('ref_axis',(1.,0.,0.));
#9129=DIRECTION('',(0.,1.,0.));
#9130=DIRECTION('center_axis',(0.,-1.,0.));
#9131=DIRECTION('ref_axis',(1.,0.,0.));
#9132=DIRECTION('center_axis',(0.,-1.,0.));
#9133=DIRECTION('ref_axis',(1.,0.,0.));
#9134=DIRECTION('center_axis',(0.,-1.,0.));
#9135=DIRECTION('ref_axis',(1.,0.,0.));
#9136=DIRECTION('',(0.,1.,0.));
#9137=DIRECTION('center_axis',(0.,-1.,0.));
#9138=DIRECTION('ref_axis',(1.,0.,0.));
#9139=DIRECTION('center_axis',(0.,1.,0.));
#9140=DIRECTION('ref_axis',(1.,0.,0.));
#9141=DIRECTION('',(-0.707106781186547,0.707106781186548,-8.65956056235493E-17));
#9142=DIRECTION('center_axis',(0.,-1.,0.));
#9143=DIRECTION('ref_axis',(1.,0.,0.));
#9144=DIRECTION('center_axis',(0.,1.,0.));
#9145=DIRECTION('ref_axis',(0.,0.,1.));
#9146=DIRECTION('center_axis',(0.,-1.,0.));
#9147=DIRECTION('ref_axis',(1.,0.,0.));
#9148=DIRECTION('center_axis',(0.,-1.,0.));
#9149=DIRECTION('ref_axis',(1.,0.,0.));
#9150=DIRECTION('',(0.,1.,0.));
#9151=DIRECTION('center_axis',(0.,-1.,0.));
#9152=DIRECTION('ref_axis',(0.,0.,-1.));
#9153=DIRECTION('center_axis',(0.,-1.,0.));
#9154=DIRECTION('ref_axis',(1.,0.,0.));
#9155=DIRECTION('center_axis',(0.,-1.,0.));
#9156=DIRECTION('ref_axis',(1.,0.,0.));
#9157=DIRECTION('',(0.707106781186547,0.707106781186548,8.65956056235493E-17));
#9158=DIRECTION('axis',(0.,0.,1.));
#9159=DIRECTION('refdir',(1.,0.,0.));
#9160=DIRECTION('center_axis',(0.,-1.,0.));
#9161=DIRECTION('ref_axis',(0.,0.,-1.));
#9162=DIRECTION('center_axis',(0.,-1.,0.));
#9163=DIRECTION('ref_axis',(1.,0.,0.));
#9164=DIRECTION('center_axis',(0.,-1.,0.));
#9165=DIRECTION('ref_axis',(1.,0.,0.));
#9166=DIRECTION('center_axis',(1.,0.,1.22464679914735E-16));
#9167=DIRECTION('ref_axis',(-1.22464679914735E-16,0.,1.));
#9168=DIRECTION('center_axis',(0.,1.,0.));
#9169=DIRECTION('ref_axis',(1.,0.,0.));
#9170=DIRECTION('center_axis',(0.,1.,0.));
#9171=DIRECTION('ref_axis',(1.,0.,0.));
#9172=DIRECTION('center_axis',(0.,-1.,0.));
#9173=DIRECTION('ref_axis',(1.,0.,0.));
#9174=DIRECTION('center_axis',(0.,-1.,0.));
#9175=DIRECTION('ref_axis',(1.,0.,0.));
#9176=DIRECTION('',(0.,1.,0.));
#9177=DIRECTION('center_axis',(0.,1.,0.));
#9178=DIRECTION('ref_axis',(0.,0.,1.));
#9179=DIRECTION('center_axis',(0.,-1.,0.));
#9180=DIRECTION('ref_axis',(1.,0.,0.));
#9181=DIRECTION('center_axis',(0.,-1.,0.));
#9182=DIRECTION('ref_axis',(1.,0.,0.));
#9183=DIRECTION('center_axis',(0.,-1.,0.));
#9184=DIRECTION('ref_axis',(1.,0.,0.));
#9185=DIRECTION('center_axis',(0.,-1.,0.));
#9186=DIRECTION('ref_axis',(1.,0.,0.));
#9187=DIRECTION('',(0.707106781186548,0.707106781186547,8.65956056235494E-17));
#9188=DIRECTION('center_axis',(0.,-1.,0.));
#9189=DIRECTION('ref_axis',(1.,0.,0.));
#9190=DIRECTION('center_axis',(0.,-1.,0.));
#9191=DIRECTION('ref_axis',(1.,0.,0.));
#9192=DIRECTION('',(0.,1.,0.));
#9193=DIRECTION('center_axis',(0.,1.,0.));
#9194=DIRECTION('ref_axis',(1.,0.,0.));
#9195=DIRECTION('center_axis',(0.,-1.,0.));
#9196=DIRECTION('ref_axis',(1.,0.,0.));
#9197=DIRECTION('',(-0.707106781186548,0.707106781186547,-8.65956056235494E-17));
#9198=DIRECTION('center_axis',(0.,-1.,0.));
#9199=DIRECTION('ref_axis',(0.,0.,-1.));
#9200=DIRECTION('center_axis',(0.,-1.,0.));
#9201=DIRECTION('ref_axis',(1.,0.,0.));
#9202=DIRECTION('',(0.,1.,0.));
#9203=DIRECTION('axis',(0.,0.,1.));
#9204=DIRECTION('refdir',(1.,0.,0.));
#9205=DIRECTION('center_axis',(0.,0.,1.));
#9206=DIRECTION('ref_axis',(1.,0.,0.));
#9207=DIRECTION('center_axis',(1.22464679914735E-16,-1.,0.));
#9208=DIRECTION('ref_axis',(-1.,-1.22464679914735E-16,0.));
#9209=DIRECTION('center_axis',(0.707106781186548,0.,0.707106781186548));
#9210=DIRECTION('ref_axis',(0.707106781186548,0.,-0.707106781186548));
#9211=DIRECTION('center_axis',(8.65956056235494E-17,-1.,-8.65956056235493E-17));
#9212=DIRECTION('ref_axis',(-0.707106781186547,-1.22464679914735E-16,0.707106781186547));
#9213=DIRECTION('center_axis',(1.,0.,0.));
#9214=DIRECTION('ref_axis',(6.12323399573676E-17,0.,-1.));
#9215=DIRECTION('center_axis',(7.49879891330929E-33,-1.,-1.22464679914735E-16));
#9216=DIRECTION('ref_axis',(-6.12323399573676E-17,-1.22464679914735E-16,
1.));
#9217=DIRECTION('center_axis',(0.707106781186548,0.,-0.707106781186548));
#9218=DIRECTION('ref_axis',(-0.707106781186548,0.,-0.707106781186548));
#9219=DIRECTION('center_axis',(-8.65956056235493E-17,-1.,-8.65956056235494E-17));
#9220=DIRECTION('ref_axis',(0.707106781186547,-1.22464679914735E-16,0.707106781186547));
#9221=DIRECTION('center_axis',(0.,0.,-1.));
#9222=DIRECTION('ref_axis',(-1.,0.,-1.22464679914735E-16));
#9223=DIRECTION('center_axis',(-1.22464679914735E-16,-1.,-1.49975978266186E-32));
#9224=DIRECTION('ref_axis',(1.,-1.22464679914735E-16,1.22464679914735E-16));
#9225=DIRECTION('center_axis',(-0.707106781186547,0.,-0.707106781186548));
#9226=DIRECTION('ref_axis',(-0.707106781186548,0.,0.707106781186547));
#9227=DIRECTION('center_axis',(-8.65956056235493E-17,-1.,8.65956056235493E-17));
#9228=DIRECTION('ref_axis',(0.707106781186548,-1.22464679914735E-16,-0.707106781186547));
#9229=DIRECTION('center_axis',(-1.,0.,0.));
#9230=DIRECTION('ref_axis',(-1.83697019872103E-16,0.,1.));
#9231=DIRECTION('center_axis',(-2.24963967399279E-32,-1.,1.22464679914735E-16));
#9232=DIRECTION('ref_axis',(1.83697019872103E-16,-1.22464679914735E-16,
-1.));
#9233=DIRECTION('center_axis',(-0.707106781186548,0.,0.707106781186548));
#9234=DIRECTION('ref_axis',(0.707106781186547,0.,0.707106781186548));
#9235=DIRECTION('center_axis',(8.65956056235493E-17,-1.,8.65956056235493E-17));
#9236=DIRECTION('ref_axis',(-0.707106781186547,-1.22464679914735E-16,-0.707106781186548));
#9237=DIRECTION('axis',(0.,0.,1.));
#9238=DIRECTION('refdir',(1.,0.,0.));
#9239=DIRECTION('center_axis',(0.,0.,1.));
#9240=DIRECTION('ref_axis',(1.,0.,0.));
#9241=DIRECTION('center_axis',(0.,-1.,0.));
#9242=DIRECTION('ref_axis',(0.,0.,-1.));
#9243=DIRECTION('center_axis',(0.,-1.,0.));
#9244=DIRECTION('ref_axis',(0.,0.,-1.));
#9245=DIRECTION('center_axis',(0.,1.,0.));
#9246=DIRECTION('ref_axis',(1.,0.,0.));
#9247=DIRECTION('center_axis',(0.,1.,0.));
#9248=DIRECTION('ref_axis',(1.,0.,0.));
#9249=DIRECTION('center_axis',(0.,1.,0.));
#9250=DIRECTION('ref_axis',(1.,0.,0.));
#9251=DIRECTION('center_axis',(0.,1.,0.));
#9252=DIRECTION('ref_axis',(1.,0.,0.));
#9253=DIRECTION('',(0.,-1.,0.));
#9254=DIRECTION('center_axis',(0.,-1.,0.));
#9255=DIRECTION('ref_axis',(1.,0.,0.));
#9256=DIRECTION('center_axis',(0.,1.,0.));
#9257=DIRECTION('ref_axis',(1.,0.,0.));
#9258=DIRECTION('center_axis',(0.,1.,0.));
#9259=DIRECTION('ref_axis',(1.,0.,0.));
#9260=DIRECTION('center_axis',(0.,1.,0.));
#9261=DIRECTION('ref_axis',(1.,0.,0.));
#9262=DIRECTION('center_axis',(0.,1.,0.));
#9263=DIRECTION('ref_axis',(1.,0.,0.));
#9264=DIRECTION('center_axis',(0.,1.,0.));
#9265=DIRECTION('ref_axis',(1.,0.,0.));
#9266=DIRECTION('center_axis',(0.,1.,0.));
#9267=DIRECTION('ref_axis',(1.,0.,0.));
#9268=DIRECTION('center_axis',(0.,-1.,0.));
#9269=DIRECTION('ref_axis',(1.,0.,0.));
#9270=DIRECTION('center_axis',(0.,-1.,0.));
#9271=DIRECTION('ref_axis',(0.,0.,-1.));
#9272=DIRECTION('center_axis',(6.12323399573677E-17,0.,1.));
#9273=DIRECTION('ref_axis',(1.,0.,0.));
#9274=DIRECTION('center_axis',(0.,-1.,0.));
#9275=DIRECTION('ref_axis',(0.,0.,-1.));
#9276=DIRECTION('center_axis',(0.,1.,0.));
#9277=DIRECTION('ref_axis',(1.,0.,0.));
#9278=DIRECTION('center_axis',(0.,-1.,0.));
#9279=DIRECTION('ref_axis',(1.,0.,0.));
#9280=DIRECTION('center_axis',(0.,-1.,0.));
#9281=DIRECTION('ref_axis',(0.,0.,-1.));
#9282=DIRECTION('center_axis',(0.,0.,1.));
#9283=DIRECTION('ref_axis',(1.,0.,0.));
#9284=DIRECTION('center_axis',(0.,-1.,0.));
#9285=DIRECTION('ref_axis',(0.,0.,-1.));
#9286=DIRECTION('center_axis',(0.,1.,0.));
#9287=DIRECTION('ref_axis',(1.,0.,0.));
#9288=DIRECTION('center_axis',(0.,-1.,0.));
#9289=DIRECTION('ref_axis',(1.,0.,0.));
#9290=DIRECTION('center_axis',(0.,-1.,0.));
#9291=DIRECTION('ref_axis',(0.,0.,-1.));
#9292=DIRECTION('center_axis',(0.,0.,1.));
#9293=DIRECTION('ref_axis',(1.,0.,0.));
#9294=DIRECTION('center_axis',(0.,-1.,0.));
#9295=DIRECTION('ref_axis',(0.,0.,-1.));
#9296=DIRECTION('center_axis',(0.,1.,0.));
#9297=DIRECTION('ref_axis',(1.,0.,0.));
#9298=DIRECTION('center_axis',(0.,-1.,0.));
#9299=DIRECTION('ref_axis',(1.,0.,0.));
#9300=DIRECTION('center_axis',(0.,-1.,0.));
#9301=DIRECTION('ref_axis',(0.,0.,-1.));
#9302=DIRECTION('center_axis',(0.,0.,1.));
#9303=DIRECTION('ref_axis',(1.,0.,0.));
#9304=DIRECTION('center_axis',(0.,-1.,0.));
#9305=DIRECTION('ref_axis',(0.,0.,-1.));
#9306=DIRECTION('center_axis',(0.,1.,0.));
#9307=DIRECTION('ref_axis',(1.,0.,0.));
#9308=DIRECTION('center_axis',(0.,-1.,0.));
#9309=DIRECTION('ref_axis',(1.,0.,0.));
#9310=DIRECTION('center_axis',(0.,-1.,0.));
#9311=DIRECTION('ref_axis',(0.,0.,-1.));
#9312=DIRECTION('center_axis',(6.12323399573676E-17,0.,1.));
#9313=DIRECTION('ref_axis',(1.,0.,0.));
#9314=DIRECTION('center_axis',(0.,-1.,0.));
#9315=DIRECTION('ref_axis',(0.,0.,-1.));
#9316=DIRECTION('center_axis',(0.,1.,0.));
#9317=DIRECTION('ref_axis',(1.,0.,0.));
#9318=DIRECTION('center_axis',(0.,-1.,0.));
#9319=DIRECTION('ref_axis',(1.,0.,0.));
#9320=DIRECTION('center_axis',(0.,-1.,0.));
#9321=DIRECTION('ref_axis',(0.,0.,-1.));
#9322=DIRECTION('center_axis',(0.,0.,1.));
#9323=DIRECTION('ref_axis',(1.,0.,0.));
#9324=DIRECTION('center_axis',(0.,-1.,0.));
#9325=DIRECTION('ref_axis',(0.,0.,-1.));
#9326=DIRECTION('center_axis',(0.,1.,0.));
#9327=DIRECTION('ref_axis',(1.,0.,0.));
#9328=DIRECTION('center_axis',(0.,1.,0.));
#9329=DIRECTION('ref_axis',(1.,0.,0.));
#9330=DIRECTION('',(0.,1.,0.));
#9331=DIRECTION('center_axis',(0.,-1.,0.));
#9332=DIRECTION('ref_axis',(1.,0.,0.));
#9333=DIRECTION('center_axis',(0.,-1.,0.));
#9334=DIRECTION('ref_axis',(1.,0.,0.));
#9335=DIRECTION('center_axis',(0.,1.,0.));
#9336=DIRECTION('ref_axis',(1.,0.,0.));
#9337=DIRECTION('center_axis',(0.,-1.,0.));
#9338=DIRECTION('ref_axis',(0.,0.,-1.));
#9339=DIRECTION('center_axis',(0.,0.,1.));
#9340=DIRECTION('ref_axis',(1.,0.,0.));
#9341=DIRECTION('center_axis',(0.,-1.,0.));
#9342=DIRECTION('ref_axis',(0.,0.,-1.));
#9343=DIRECTION('center_axis',(0.,-1.,0.));
#9344=DIRECTION('ref_axis',(-1.,0.,0.));
#9345=DIRECTION('center_axis',(0.,1.,0.));
#9346=DIRECTION('ref_axis',(1.,0.,0.));
#9347=DIRECTION('axis',(0.,0.,1.));
#9348=DIRECTION('refdir',(1.,0.,0.));
#9349=DIRECTION('center_axis',(0.,1.,0.));
#9350=DIRECTION('ref_axis',(0.,0.,1.));
#9351=DIRECTION('center_axis',(0.,-1.,0.));
#9352=DIRECTION('ref_axis',(1.,0.,0.));
#9353=DIRECTION('center_axis',(0.,-1.,0.));
#9354=DIRECTION('ref_axis',(1.,0.,0.));
#9355=DIRECTION('center_axis',(0.,-1.,0.));
#9356=DIRECTION('ref_axis',(1.,0.,0.));
#9357=DIRECTION('center_axis',(0.,-1.,0.));
#9358=DIRECTION('ref_axis',(1.,0.,0.));
#9359=DIRECTION('',(0.,1.,0.));
#9360=DIRECTION('center_axis',(0.,-1.,0.));
#9361=DIRECTION('ref_axis',(0.,0.,-1.));
#9362=DIRECTION('center_axis',(0.,-1.,0.));
#9363=DIRECTION('ref_axis',(1.,0.,0.));
#9364=DIRECTION('center_axis',(0.,-1.,0.));
#9365=DIRECTION('ref_axis',(1.,0.,0.));
#9366=DIRECTION('',(0.,1.,0.));
#9367=DIRECTION('center_axis',(0.,1.,0.));
#9368=DIRECTION('ref_axis',(0.,0.,1.));
#9369=DIRECTION('center_axis',(0.,-1.,0.));
#9370=DIRECTION('ref_axis',(1.,0.,0.));
#9371=DIRECTION('center_axis',(0.,-1.,0.));
#9372=DIRECTION('ref_axis',(1.,0.,0.));
#9373=DIRECTION('center_axis',(0.,-1.,0.));
#9374=DIRECTION('ref_axis',(1.,0.,0.));
#9375=DIRECTION('center_axis',(0.,-1.,0.));
#9376=DIRECTION('ref_axis',(1.,0.,0.));
#9377=DIRECTION('',(0.,1.,0.));
#9378=DIRECTION('center_axis',(0.,-1.,0.));
#9379=DIRECTION('ref_axis',(0.,0.,-1.));
#9380=DIRECTION('center_axis',(0.,-1.,0.));
#9381=DIRECTION('ref_axis',(1.,0.,0.));
#9382=DIRECTION('center_axis',(0.,-1.,0.));
#9383=DIRECTION('ref_axis',(1.,0.,0.));
#9384=DIRECTION('',(0.,1.,0.));
#9385=DIRECTION('',(0.,0.,1.));
#9386=DIRECTION('',(1.,0.,0.));
#9387=DIRECTION('',(0.,0.,1.));
#9388=DIRECTION('',(1.,0.,0.));
#9389=DIRECTION('',(0.,0.,1.));
#9390=DIRECTION('',(1.,0.,0.));
#9391=DIRECTION('',(0.,0.,1.));
#9392=DIRECTION('',(1.,0.,0.));
#9393=DIRECTION('',(0.,0.,1.));
#9394=DIRECTION('',(1.,0.,0.));
#9395=DIRECTION('axis',(0.,0.,1.));
#9396=DIRECTION('refdir',(1.,0.,0.));
#9397=DIRECTION('center_axis',(0.,1.,0.));
#9398=DIRECTION('ref_axis',(1.,0.,0.));
#9399=DIRECTION('center_axis',(0.,-1.,0.));
#9400=DIRECTION('ref_axis',(1.,0.,0.));
#9401=DIRECTION('',(0.,-1.,0.));
#9402=DIRECTION('center_axis',(0.,-1.,0.));
#9403=DIRECTION('ref_axis',(1.,0.,0.));
#9404=DIRECTION('center_axis',(0.,1.,0.));
#9405=DIRECTION('ref_axis',(1.,0.,0.));
#9406=DIRECTION('center_axis',(0.,1.,0.));
#9407=DIRECTION('ref_axis',(1.,0.,0.));
#9408=DIRECTION('',(0.,-1.,0.));
#9409=DIRECTION('center_axis',(0.,1.,0.));
#9410=DIRECTION('ref_axis',(1.,0.,0.));
#9411=DIRECTION('center_axis',(0.,1.,0.));
#9412=DIRECTION('ref_axis',(1.,0.,0.));
#9413=DIRECTION('center_axis',(0.,1.,0.));
#9414=DIRECTION('ref_axis',(1.,0.,0.));
#9415=DIRECTION('axis',(0.,0.,1.));
#9416=DIRECTION('refdir',(1.,0.,0.));
#9417=DIRECTION('center_axis',(0.,1.,0.));
#9418=DIRECTION('ref_axis',(1.,0.,0.));
#9419=DIRECTION('center_axis',(0.,-1.,0.));
#9420=DIRECTION('ref_axis',(1.,0.,0.));
#9421=DIRECTION('',(0.,-1.,0.));
#9422=DIRECTION('center_axis',(0.,-1.,0.));
#9423=DIRECTION('ref_axis',(1.,0.,0.));
#9424=DIRECTION('center_axis',(0.,1.,0.));
#9425=DIRECTION('ref_axis',(1.,0.,0.));
#9426=DIRECTION('center_axis',(0.,1.,0.));
#9427=DIRECTION('ref_axis',(1.,0.,0.));
#9428=DIRECTION('',(0.,-1.,0.));
#9429=DIRECTION('center_axis',(0.,1.,0.));
#9430=DIRECTION('ref_axis',(1.,0.,0.));
#9431=DIRECTION('center_axis',(0.,1.,0.));
#9432=DIRECTION('ref_axis',(1.,0.,0.));
#9433=DIRECTION('center_axis',(0.,1.,0.));
#9434=DIRECTION('ref_axis',(1.,0.,0.));
#9435=DIRECTION('axis',(0.,0.,1.));
#9436=DIRECTION('refdir',(1.,0.,0.));
#9437=DIRECTION('center_axis',(0.,1.,0.));
#9438=DIRECTION('ref_axis',(1.,0.,0.));
#9439=DIRECTION('center_axis',(0.,-1.,0.));
#9440=DIRECTION('ref_axis',(1.,0.,0.));
#9441=DIRECTION('',(0.,-1.,0.));
#9442=DIRECTION('center_axis',(0.,-1.,0.));
#9443=DIRECTION('ref_axis',(1.,0.,0.));
#9444=DIRECTION('center_axis',(0.,1.,0.));
#9445=DIRECTION('ref_axis',(1.,0.,0.));
#9446=DIRECTION('center_axis',(0.,1.,0.));
#9447=DIRECTION('ref_axis',(1.,0.,0.));
#9448=DIRECTION('',(0.,-1.,0.));
#9449=DIRECTION('center_axis',(0.,1.,0.));
#9450=DIRECTION('ref_axis',(1.,0.,0.));
#9451=DIRECTION('center_axis',(0.,1.,0.));
#9452=DIRECTION('ref_axis',(1.,0.,0.));
#9453=DIRECTION('center_axis',(0.,1.,0.));
#9454=DIRECTION('ref_axis',(1.,0.,0.));
#9455=DIRECTION('',(0.,0.,1.));
#9456=DIRECTION('',(1.,0.,0.));
#9457=DIRECTION('',(0.,0.,1.));
#9458=DIRECTION('',(1.,0.,0.));
#9459=DIRECTION('',(0.,0.,1.));
#9460=DIRECTION('',(1.,0.,0.));
#9461=DIRECTION('',(0.,0.,1.));
#9462=DIRECTION('',(1.,0.,0.));
#9463=DIRECTION('',(0.,0.,1.));
#9464=DIRECTION('',(1.,0.,0.));
#9465=DIRECTION('',(0.,0.,1.));
#9466=DIRECTION('',(1.,0.,0.));
#9467=DIRECTION('',(0.,0.,1.));
#9468=DIRECTION('',(1.,0.,0.));
#9469=DIRECTION('',(0.,0.,1.));
#9470=DIRECTION('',(1.,0.,0.));
#9471=DIRECTION('',(0.0748447804833849,0.,0.99719519595433));
#9472=DIRECTION('',(0.99719519595433,0.,-0.0748447804833849));
#9473=DIRECTION('',(-0.0516120301317117,-1.16062088058833E-17,0.998667211009595));
#9474=DIRECTION('',(0.998667211009596,2.22044604925032E-16,0.0516120301317118));
#9475=CARTESIAN_POINT('',(0.,0.,0.));
#9476=CARTESIAN_POINT('',(0.,0.,0.));
#9477=CARTESIAN_POINT('',(0.,0.,0.));
#9478=CARTESIAN_POINT('Origin',(-0.1,0.82,-0.3));
#9479=CARTESIAN_POINT('',(0.,0.82,-0.3));
#9480=CARTESIAN_POINT('',(0.,1.,-0.3));
#9481=CARTESIAN_POINT('',(0.,0.41,-0.3));
#9482=CARTESIAN_POINT('',(40.,0.82,-0.3));
#9483=CARTESIAN_POINT('',(-0.1,0.82,-0.3));
#9484=CARTESIAN_POINT('',(40.,1.,-0.3));
#9485=CARTESIAN_POINT('',(40.,0.41,-0.3));
#9486=CARTESIAN_POINT('',(-0.05,1.,-0.3));
#9487=CARTESIAN_POINT('Origin',(-0.1,0.82,-0.55));
#9488=CARTESIAN_POINT('',(0.,0.82,-0.55));
#9489=CARTESIAN_POINT('',(0.,0.82,-0.275));
#9490=CARTESIAN_POINT('',(40.,0.82,-0.55));
#9491=CARTESIAN_POINT('',(-0.1,0.82,-0.55));
#9492=CARTESIAN_POINT('',(40.,0.82,-0.275));
#9493=CARTESIAN_POINT('Origin',(-0.1,0.67,-0.55));
#9494=CARTESIAN_POINT('',(0.,0.67,-0.55));
#9495=CARTESIAN_POINT('',(0.,0.335,-0.55));
#9496=CARTESIAN_POINT('',(40.,0.67,-0.55));
#9497=CARTESIAN_POINT('',(-0.1,0.67,-0.55));
#9498=CARTESIAN_POINT('',(40.,0.335,-0.55));
#9499=CARTESIAN_POINT('Origin',(-0.1,0.42,-0.3));
#9500=CARTESIAN_POINT('',(0.,0.42,-0.3));
#9501=CARTESIAN_POINT('',(0.,0.24,-0.12));
#9502=CARTESIAN_POINT('',(40.,0.42,-0.3));
#9503=CARTESIAN_POINT('',(-0.1,0.42,-0.3));
#9504=CARTESIAN_POINT('',(40.,0.24,-0.12));
#9505=CARTESIAN_POINT('Origin',(-0.1,0.42,0.3));
#9506=CARTESIAN_POINT('',(0.,0.42,0.3));
#9507=CARTESIAN_POINT('',(0.,0.42,0.15));
#9508=CARTESIAN_POINT('',(40.,0.42,0.3));
#9509=CARTESIAN_POINT('',(-0.1,0.42,0.3));
#9510=CARTESIAN_POINT('',(40.,0.42,0.15));
#9511=CARTESIAN_POINT('Origin',(-0.1,0.67,0.55));
#9512=CARTESIAN_POINT('',(0.,0.67,0.55));
#9513=CARTESIAN_POINT('',(6.93889390390723E-18,0.365,0.245));
#9514=CARTESIAN_POINT('',(40.,0.67,0.55));
#9515=CARTESIAN_POINT('',(-0.1,0.67,0.55));
#9516=CARTESIAN_POINT('',(40.,0.365,0.245));
#9517=CARTESIAN_POINT('Origin',(-0.1,0.82,0.55));
#9518=CARTESIAN_POINT('',(0.,0.82,0.55));
#9519=CARTESIAN_POINT('',(0.,0.41,0.55));
#9520=CARTESIAN_POINT('',(40.,0.82,0.55));
#9521=CARTESIAN_POINT('',(-0.1,0.82,0.55));
#9522=CARTESIAN_POINT('',(40.,0.41,0.55));
#9523=CARTESIAN_POINT('Origin',(-0.1,0.82,0.3));
#9524=CARTESIAN_POINT('',(0.,0.82,0.3));
#9525=CARTESIAN_POINT('',(0.,0.82,0.15));
#9526=CARTESIAN_POINT('',(40.,0.82,0.3));
#9527=CARTESIAN_POINT('',(-0.1,0.82,0.3));
#9528=CARTESIAN_POINT('',(40.,0.82,0.15));
#9529=CARTESIAN_POINT('Origin',(-0.1,1.05,0.3));
#9530=CARTESIAN_POINT('',(0.,1.,0.3));
#9531=CARTESIAN_POINT('',(0.,0.525,0.3));
#9532=CARTESIAN_POINT('',(40.,1.,0.3));
#9533=CARTESIAN_POINT('',(-0.05,1.,0.3));
#9534=CARTESIAN_POINT('',(40.,0.525,0.3));
#9535=CARTESIAN_POINT('Origin',(-0.1,-0.3,-0.82));
#9536=CARTESIAN_POINT('',(0.,-0.3,-0.82));
#9537=CARTESIAN_POINT('',(0.,-0.3,-1.));
#9538=CARTESIAN_POINT('',(0.,-0.3,-0.41));
#9539=CARTESIAN_POINT('',(40.,-0.3,-0.82));
#9540=CARTESIAN_POINT('',(-0.1,-0.3,-0.82));
#9541=CARTESIAN_POINT('',(40.,-0.3,-1.));
#9542=CARTESIAN_POINT('',(40.,-0.3,-0.41));
#9543=CARTESIAN_POINT('',(-0.05,-0.3,-1.));
#9544=CARTESIAN_POINT('Origin',(-0.1,-0.55,-0.82));
#9545=CARTESIAN_POINT('',(0.,-0.55,-0.82));
#9546=CARTESIAN_POINT('',(0.,-0.275,-0.82));
#9547=CARTESIAN_POINT('',(40.,-0.55,-0.82));
#9548=CARTESIAN_POINT('',(-0.1,-0.55,-0.82));
#9549=CARTESIAN_POINT('',(40.,-0.275,-0.82));
#9550=CARTESIAN_POINT('Origin',(-0.1,-0.55,-0.67));
#9551=CARTESIAN_POINT('',(0.,-0.55,-0.67));
#9552=CARTESIAN_POINT('',(0.,-0.55,-0.335));
#9553=CARTESIAN_POINT('',(40.,-0.55,-0.67));
#9554=CARTESIAN_POINT('',(-0.1,-0.55,-0.67));
#9555=CARTESIAN_POINT('',(40.,-0.55,-0.335));
#9556=CARTESIAN_POINT('Origin',(-0.1,-0.3,-0.42));
#9557=CARTESIAN_POINT('',(0.,-0.3,-0.42));
#9558=CARTESIAN_POINT('',(0.,-0.12,-0.24));
#9559=CARTESIAN_POINT('',(40.,-0.3,-0.42));
#9560=CARTESIAN_POINT('',(-0.1,-0.3,-0.42));
#9561=CARTESIAN_POINT('',(40.,-0.12,-0.24));
#9562=CARTESIAN_POINT('Origin',(-0.1,0.3,-0.42));
#9563=CARTESIAN_POINT('',(0.,0.3,-0.42));
#9564=CARTESIAN_POINT('',(0.,0.15,-0.42));
#9565=CARTESIAN_POINT('',(40.,0.3,-0.42));
#9566=CARTESIAN_POINT('',(-0.1,0.3,-0.42));
#9567=CARTESIAN_POINT('',(40.,0.15,-0.42));
#9568=CARTESIAN_POINT('Origin',(-0.1,0.55,-0.67));
#9569=CARTESIAN_POINT('',(0.,0.55,-0.67));
#9570=CARTESIAN_POINT('',(0.,0.245,-0.365));
#9571=CARTESIAN_POINT('',(40.,0.55,-0.67));
#9572=CARTESIAN_POINT('',(-0.1,0.55,-0.67));
#9573=CARTESIAN_POINT('',(40.,0.245,-0.365));
#9574=CARTESIAN_POINT('Origin',(-0.1,0.55,-0.82));
#9575=CARTESIAN_POINT('',(0.,0.55,-0.82));
#9576=CARTESIAN_POINT('',(0.,0.55,-0.41));
#9577=CARTESIAN_POINT('',(40.,0.55,-0.82));
#9578=CARTESIAN_POINT('',(-0.1,0.55,-0.82));
#9579=CARTESIAN_POINT('',(40.,0.55,-0.41));
#9580=CARTESIAN_POINT('Origin',(-0.1,0.3,-0.82));
#9581=CARTESIAN_POINT('',(0.,0.3,-0.82));
#9582=CARTESIAN_POINT('',(0.,0.15,-0.82));
#9583=CARTESIAN_POINT('',(40.,0.3,-0.82));
#9584=CARTESIAN_POINT('',(-0.1,0.3,-0.82));
#9585=CARTESIAN_POINT('',(40.,0.15,-0.82));
#9586=CARTESIAN_POINT('Origin',(-0.1,0.3,-1.05));
#9587=CARTESIAN_POINT('',(0.,0.3,-1.));
#9588=CARTESIAN_POINT('',(0.,0.3,-0.525));
#9589=CARTESIAN_POINT('',(40.,0.3,-1.));
#9590=CARTESIAN_POINT('',(-0.05,0.3,-1.));
#9591=CARTESIAN_POINT('',(40.,0.3,-0.525));
#9592=CARTESIAN_POINT('Origin',(-0.1,-0.82,0.3));
#9593=CARTESIAN_POINT('',(0.,-0.82,0.3));
#9594=CARTESIAN_POINT('',(0.,-1.,0.3));
#9595=CARTESIAN_POINT('',(0.,-0.41,0.3));
#9596=CARTESIAN_POINT('',(40.,-0.82,0.3));
#9597=CARTESIAN_POINT('',(-0.1,-0.82,0.3));
#9598=CARTESIAN_POINT('',(40.,-1.,0.3));
#9599=CARTESIAN_POINT('',(40.,-0.41,0.3));
#9600=CARTESIAN_POINT('',(-0.05,-1.,0.3));
#9601=CARTESIAN_POINT('Origin',(-0.1,-0.82,0.55));
#9602=CARTESIAN_POINT('',(0.,-0.82,0.55));
#9603=CARTESIAN_POINT('',(0.,-0.82,0.275));
#9604=CARTESIAN_POINT('',(40.,-0.82,0.55));
#9605=CARTESIAN_POINT('',(-0.1,-0.82,0.55));
#9606=CARTESIAN_POINT('',(40.,-0.82,0.275));
#9607=CARTESIAN_POINT('Origin',(-0.1,-0.67,0.55));
#9608=CARTESIAN_POINT('',(0.,-0.67,0.55));
#9609=CARTESIAN_POINT('',(0.,-0.335,0.55));
#9610=CARTESIAN_POINT('',(40.,-0.67,0.55));
#9611=CARTESIAN_POINT('',(-0.1,-0.67,0.55));
#9612=CARTESIAN_POINT('',(40.,-0.335,0.55));
#9613=CARTESIAN_POINT('Origin',(-0.1,-0.42,0.3));
#9614=CARTESIAN_POINT('',(0.,-0.42,0.3));
#9615=CARTESIAN_POINT('',(-6.93889390390723E-18,-0.24,0.12));
#9616=CARTESIAN_POINT('',(40.,-0.42,0.3));
#9617=CARTESIAN_POINT('',(-0.1,-0.42,0.3));
#9618=CARTESIAN_POINT('',(40.,-0.24,0.12));
#9619=CARTESIAN_POINT('Origin',(-0.1,-0.42,-0.3));
#9620=CARTESIAN_POINT('',(0.,-0.42,-0.3));
#9621=CARTESIAN_POINT('',(0.,-0.42,-0.15));
#9622=CARTESIAN_POINT('',(40.,-0.42,-0.3));
#9623=CARTESIAN_POINT('',(-0.1,-0.42,-0.3));
#9624=CARTESIAN_POINT('',(40.,-0.42,-0.15));
#9625=CARTESIAN_POINT('Origin',(-0.1,-0.67,-0.55));
#9626=CARTESIAN_POINT('',(0.,-0.67,-0.55));
#9627=CARTESIAN_POINT('',(0.,-0.365,-0.245));
#9628=CARTESIAN_POINT('',(40.,-0.67,-0.55));
#9629=CARTESIAN_POINT('',(-0.1,-0.67,-0.55));
#9630=CARTESIAN_POINT('',(40.,-0.365,-0.245));
#9631=CARTESIAN_POINT('Origin',(-0.1,-0.82,-0.55));
#9632=CARTESIAN_POINT('',(0.,-0.82,-0.55));
#9633=CARTESIAN_POINT('',(0.,-0.41,-0.55));
#9634=CARTESIAN_POINT('',(40.,-0.82,-0.55));
#9635=CARTESIAN_POINT('',(-0.1,-0.82,-0.55));
#9636=CARTESIAN_POINT('',(40.,-0.41,-0.55));
#9637=CARTESIAN_POINT('Origin',(-0.1,-0.82,-0.3));
#9638=CARTESIAN_POINT('',(0.,-0.82,-0.3));
#9639=CARTESIAN_POINT('',(0.,-0.82,-0.15));
#9640=CARTESIAN_POINT('',(40.,-0.82,-0.3));
#9641=CARTESIAN_POINT('',(-0.1,-0.82,-0.3));
#9642=CARTESIAN_POINT('',(40.,-0.82,-0.15));
#9643=CARTESIAN_POINT('Origin',(-0.1,-1.05,-0.3));
#9644=CARTESIAN_POINT('',(0.,-1.,-0.3));
#9645=CARTESIAN_POINT('',(0.,-0.525,-0.3));
#9646=CARTESIAN_POINT('',(40.,-1.,-0.3));
#9647=CARTESIAN_POINT('',(-0.05,-1.,-0.3));
#9648=CARTESIAN_POINT('',(40.,-0.525,-0.3));
#9649=CARTESIAN_POINT('Origin',(-0.1,0.3,0.82));
#9650=CARTESIAN_POINT('',(0.,0.3,0.82));
#9651=CARTESIAN_POINT('',(0.,0.3,1.));
#9652=CARTESIAN_POINT('',(0.,0.3,0.41));
#9653=CARTESIAN_POINT('',(40.,0.3,0.82));
#9654=CARTESIAN_POINT('',(-0.1,0.3,0.82));
#9655=CARTESIAN_POINT('',(40.,0.3,1.));
#9656=CARTESIAN_POINT('',(40.,0.3,0.41));
#9657=CARTESIAN_POINT('',(-0.05,0.3,1.));
#9658=CARTESIAN_POINT('Origin',(-0.1,0.55,0.82));
#9659=CARTESIAN_POINT('',(0.,0.55,0.82));
#9660=CARTESIAN_POINT('',(0.,0.275,0.82));
#9661=CARTESIAN_POINT('',(40.,0.55,0.82));
#9662=CARTESIAN_POINT('',(-0.1,0.55,0.82));
#9663=CARTESIAN_POINT('',(40.,0.275,0.82));
#9664=CARTESIAN_POINT('Origin',(-0.1,0.55,0.67));
#9665=CARTESIAN_POINT('',(0.,0.55,0.67));
#9666=CARTESIAN_POINT('',(0.,0.55,0.335));
#9667=CARTESIAN_POINT('',(40.,0.55,0.67));
#9668=CARTESIAN_POINT('',(-0.1,0.55,0.67));
#9669=CARTESIAN_POINT('',(40.,0.55,0.335));
#9670=CARTESIAN_POINT('Origin',(-0.1,0.3,0.42));
#9671=CARTESIAN_POINT('',(0.,0.3,0.42));
#9672=CARTESIAN_POINT('',(6.93889390390723E-18,0.12,0.24));
#9673=CARTESIAN_POINT('',(40.,0.3,0.42));
#9674=CARTESIAN_POINT('',(-0.1,0.3,0.42));
#9675=CARTESIAN_POINT('',(40.,0.12,0.24));
#9676=CARTESIAN_POINT('Origin',(-0.1,-0.3,0.42));
#9677=CARTESIAN_POINT('',(0.,-0.3,0.42));
#9678=CARTESIAN_POINT('',(0.,-0.15,0.42));
#9679=CARTESIAN_POINT('',(40.,-0.3,0.42));
#9680=CARTESIAN_POINT('',(-0.1,-0.3,0.42));
#9681=CARTESIAN_POINT('',(40.,-0.15,0.42));
#9682=CARTESIAN_POINT('Origin',(-0.1,-0.55,0.67));
#9683=CARTESIAN_POINT('',(0.,-0.55,0.67));
#9684=CARTESIAN_POINT('',(6.93889390390723E-18,-0.245,0.365));
#9685=CARTESIAN_POINT('',(40.,-0.55,0.67));
#9686=CARTESIAN_POINT('',(-0.1,-0.55,0.67));
#9687=CARTESIAN_POINT('',(40.,-0.245,0.365));
#9688=CARTESIAN_POINT('Origin',(-0.1,-0.55,0.82));
#9689=CARTESIAN_POINT('',(0.,-0.55,0.82));
#9690=CARTESIAN_POINT('',(0.,-0.55,0.41));
#9691=CARTESIAN_POINT('',(40.,-0.55,0.82));
#9692=CARTESIAN_POINT('',(-0.1,-0.55,0.82));
#9693=CARTESIAN_POINT('',(40.,-0.55,0.41));
#9694=CARTESIAN_POINT('Origin',(-0.1,-0.3,0.82));
#9695=CARTESIAN_POINT('',(0.,-0.3,0.82));
#9696=CARTESIAN_POINT('',(0.,-0.15,0.82));
#9697=CARTESIAN_POINT('',(40.,-0.3,0.82));
#9698=CARTESIAN_POINT('',(-0.1,-0.3,0.82));
#9699=CARTESIAN_POINT('',(40.,-0.15,0.82));
#9700=CARTESIAN_POINT('Origin',(-0.1,-0.3,1.05));
#9701=CARTESIAN_POINT('',(0.,-0.3,1.));
#9702=CARTESIAN_POINT('',(0.,-0.3,0.525));
#9703=CARTESIAN_POINT('',(40.,-0.3,1.));
#9704=CARTESIAN_POINT('',(-0.05,-0.3,1.));
#9705=CARTESIAN_POINT('',(40.,-0.3,0.525));
#9706=CARTESIAN_POINT('Origin',(-0.1,0.,0.));
#9707=CARTESIAN_POINT('',(0.,-2.57175827820944E-17,0.21));
#9708=CARTESIAN_POINT('Origin',(0.,0.,0.));
#9709=CARTESIAN_POINT('',(40.,2.57175827820944E-17,0.21));
#9710=CARTESIAN_POINT('',(-0.1,-2.57175827820944E-17,0.21));
#9711=CARTESIAN_POINT('Origin',(40.,0.,0.));
#9712=CARTESIAN_POINT('Origin',(0.,1.,-1.));
#9713=CARTESIAN_POINT('',(0.,1.,1.));
#9714=CARTESIAN_POINT('',(0.,1.,-1.));
#9715=CARTESIAN_POINT('',(40.,1.,1.));
#9716=CARTESIAN_POINT('',(0.,1.,1.));
#9717=CARTESIAN_POINT('',(40.,1.,-1.));
#9718=CARTESIAN_POINT('Origin',(0.,1.,-1.));
#9719=CARTESIAN_POINT('',(40.,1.,-1.));
#9720=CARTESIAN_POINT('',(40.,1.,-1.));
#9721=CARTESIAN_POINT('',(0.,1.,-1.));
#9722=CARTESIAN_POINT('',(0.,1.,-1.));
#9723=CARTESIAN_POINT('',(0.,1.,-1.));
#9724=CARTESIAN_POINT('Origin',(0.,-1.,-1.));
#9725=CARTESIAN_POINT('',(0.,-1.,-1.));
#9726=CARTESIAN_POINT('',(40.,-1.,-1.));
#9727=CARTESIAN_POINT('Origin',(0.,-1.,-1.));
#9728=CARTESIAN_POINT('',(40.,-1.,-1.));
#9729=CARTESIAN_POINT('',(40.,-1.,-1.));
#9730=CARTESIAN_POINT('',(0.,-1.,-1.));
#9731=CARTESIAN_POINT('',(0.,-1.,-1.));
#9732=CARTESIAN_POINT('',(0.,-1.,-1.));
#9733=CARTESIAN_POINT('Origin',(0.,-1.,1.));
#9734=CARTESIAN_POINT('',(0.,-1.,1.));
#9735=CARTESIAN_POINT('',(40.,-1.,1.));
#9736=CARTESIAN_POINT('Origin',(0.,-1.,1.));
#9737=CARTESIAN_POINT('',(40.,-1.,1.));
#9738=CARTESIAN_POINT('',(40.,-1.,1.));
#9739=CARTESIAN_POINT('',(0.,-1.,1.));
#9740=CARTESIAN_POINT('',(0.,-1.,1.));
#9741=CARTESIAN_POINT('',(0.,-1.,1.));
#9742=CARTESIAN_POINT('Origin',(0.,1.,1.));
#9743=CARTESIAN_POINT('',(0.,1.,1.));
#9744=CARTESIAN_POINT('',(40.,1.,1.));
#9745=CARTESIAN_POINT('Origin',(0.,1.,1.));
#9746=CARTESIAN_POINT('',(40.,1.,1.));
#9747=CARTESIAN_POINT('',(0.,1.,1.));
#9748=CARTESIAN_POINT('Origin',(40.,0.,0.));
#9749=CARTESIAN_POINT('Origin',(0.,0.,0.));
#9750=CARTESIAN_POINT('',(0.,0.,0.));
#9751=CARTESIAN_POINT('Origin',(5.,-1.2,1.9));
#9752=CARTESIAN_POINT('',(4.79,-1.2,2.));
#9753=CARTESIAN_POINT('Origin',(5.,-1.2,2.));
#9754=CARTESIAN_POINT('',(4.79,-1.2,2.8));
#9755=CARTESIAN_POINT('',(4.79,-1.2,1.9));
#9756=CARTESIAN_POINT('Origin',(5.,-1.2,2.8));
#9757=CARTESIAN_POINT('Origin',(5.,1.2,1.9));
#9758=CARTESIAN_POINT('',(4.79,1.2,2.));
#9759=CARTESIAN_POINT('Origin',(5.,1.2,2.));
#9760=CARTESIAN_POINT('',(4.79,1.2,2.8));
#9761=CARTESIAN_POINT('',(4.79,1.2,1.9));
#9762=CARTESIAN_POINT('Origin',(5.,1.2,2.8));
#9763=CARTESIAN_POINT('Origin',(-3.5,7.5,1.9));
#9764=CARTESIAN_POINT('',(-3.75,7.5,2.));
#9765=CARTESIAN_POINT('Origin',(-3.5,7.5,2.));
#9766=CARTESIAN_POINT('',(-3.75,7.5,2.8));
#9767=CARTESIAN_POINT('',(-3.75,7.5,1.9));
#9768=CARTESIAN_POINT('Origin',(-3.5,7.5,2.8));
#9769=CARTESIAN_POINT('Origin',(3.5,7.5,1.9));
#9770=CARTESIAN_POINT('',(3.25,7.5,2.));
#9771=CARTESIAN_POINT('Origin',(3.5,7.5,2.));
#9772=CARTESIAN_POINT('',(3.25,7.5,2.8));
#9773=CARTESIAN_POINT('',(3.25,7.5,1.9));
#9774=CARTESIAN_POINT('Origin',(3.5,7.5,2.8));
#9775=CARTESIAN_POINT('Origin',(-3.5,-12.5,1.9));
#9776=CARTESIAN_POINT('',(-3.75,-12.5,2.));
#9777=CARTESIAN_POINT('Origin',(-3.5,-12.5,2.));
#9778=CARTESIAN_POINT('',(-3.75,-12.5,2.8));
#9779=CARTESIAN_POINT('',(-3.75,-12.5,1.9));
#9780=CARTESIAN_POINT('Origin',(-3.5,-12.5,2.8));
#9781=CARTESIAN_POINT('Origin',(3.5,-12.5,1.9));
#9782=CARTESIAN_POINT('',(3.25,-12.5,2.));
#9783=CARTESIAN_POINT('Origin',(3.5,-12.5,2.));
#9784=CARTESIAN_POINT('',(3.25,-12.5,2.8));
#9785=CARTESIAN_POINT('',(3.25,-12.5,1.9));
#9786=CARTESIAN_POINT('Origin',(3.5,-12.5,2.8));
#9787=CARTESIAN_POINT('Origin',(4.,4.,1.9));
#9788=CARTESIAN_POINT('',(3.725,4.,2.));
#9789=CARTESIAN_POINT('Origin',(4.,4.,2.));
#9790=CARTESIAN_POINT('',(3.725,4.,2.8));
#9791=CARTESIAN_POINT('',(3.725,4.,1.9));
#9792=CARTESIAN_POINT('Origin',(4.,4.,2.8));
#9793=CARTESIAN_POINT('Origin',(-4.,-15.,1.9));
#9794=CARTESIAN_POINT('',(-4.275,-15.,2.));
#9795=CARTESIAN_POINT('Origin',(-4.,-15.,2.));
#9796=CARTESIAN_POINT('',(-4.275,-15.,2.8));
#9797=CARTESIAN_POINT('',(-4.275,-15.,1.9));
#9798=CARTESIAN_POINT('Origin',(-4.,-15.,2.8));
#9799=CARTESIAN_POINT('Origin',(-4.,4.,1.9));
#9800=CARTESIAN_POINT('',(-4.275,4.,2.));
#9801=CARTESIAN_POINT('Origin',(-4.,4.,2.));
#9802=CARTESIAN_POINT('',(-4.275,4.,2.8));
#9803=CARTESIAN_POINT('',(-4.275,4.,1.9));
#9804=CARTESIAN_POINT('Origin',(-4.,4.,2.8));
#9805=CARTESIAN_POINT('Origin',(-4.,15.,1.9));
#9806=CARTESIAN_POINT('',(-4.275,15.,2.));
#9807=CARTESIAN_POINT('Origin',(-4.,15.,2.));
#9808=CARTESIAN_POINT('',(-4.275,15.,2.8));
#9809=CARTESIAN_POINT('',(-4.275,15.,1.9));
#9810=CARTESIAN_POINT('Origin',(-4.,15.,2.8));
#9811=CARTESIAN_POINT('Origin',(4.,-15.,1.9));
#9812=CARTESIAN_POINT('',(3.725,-15.,2.));
#9813=CARTESIAN_POINT('Origin',(4.,-15.,2.));
#9814=CARTESIAN_POINT('',(3.725,-15.,2.8));
#9815=CARTESIAN_POINT('',(3.725,-15.,1.9));
#9816=CARTESIAN_POINT('Origin',(4.,-15.,2.8));
#9817=CARTESIAN_POINT('Origin',(4.,15.,1.9));
#9818=CARTESIAN_POINT('',(3.725,15.,2.));
#9819=CARTESIAN_POINT('Origin',(4.,15.,2.));
#9820=CARTESIAN_POINT('',(3.725,15.,2.8));
#9821=CARTESIAN_POINT('',(3.725,15.,1.9));
#9822=CARTESIAN_POINT('Origin',(4.,15.,2.8));
#9823=CARTESIAN_POINT('Origin',(6.,18.,2.));
#9824=CARTESIAN_POINT('',(6.,18.,2.));
#9825=CARTESIAN_POINT('',(-6.,18.,2.));
#9826=CARTESIAN_POINT('',(6.,18.,2.));
#9827=CARTESIAN_POINT('',(-6.,18.,2.8));
#9828=CARTESIAN_POINT('',(-6.,18.,2.));
#9829=CARTESIAN_POINT('',(6.,18.,2.8));
#9830=CARTESIAN_POINT('',(6.,18.,2.8));
#9831=CARTESIAN_POINT('',(6.,18.,2.));
#9832=CARTESIAN_POINT('Origin',(6.,-18.,2.));
#9833=CARTESIAN_POINT('',(6.,-18.,2.));
#9834=CARTESIAN_POINT('',(6.,-18.,2.));
#9835=CARTESIAN_POINT('',(6.,-18.,2.8));
#9836=CARTESIAN_POINT('',(6.,-18.,2.8));
#9837=CARTESIAN_POINT('',(6.,-18.,2.));
#9838=CARTESIAN_POINT('Origin',(-6.,-18.,2.));
#9839=CARTESIAN_POINT('',(-6.,-18.,2.));
#9840=CARTESIAN_POINT('',(-6.,-18.,2.));
#9841=CARTESIAN_POINT('',(-6.,-18.,2.8));
#9842=CARTESIAN_POINT('',(-6.,-18.,2.8));
#9843=CARTESIAN_POINT('',(-6.,-18.,2.));
#9844=CARTESIAN_POINT('Origin',(-6.,18.,2.));
#9845=CARTESIAN_POINT('',(-6.,18.,2.));
#9846=CARTESIAN_POINT('',(-6.,18.,2.8));
#9847=CARTESIAN_POINT('Origin',(0.,0.,2.8));
#9848=CARTESIAN_POINT('Origin',(0.,0.,2.));
#9849=CARTESIAN_POINT('',(0.,0.,0.));
#9850=CARTESIAN_POINT('Origin',(0.,0.395,0.25));
#9851=CARTESIAN_POINT('',(-0.5,0.3,0.25));
#9852=CARTESIAN_POINT('',(0.5,0.3,0.25));
#9853=CARTESIAN_POINT('',(0.25,0.3,0.25));
#9854=CARTESIAN_POINT('',(-0.5,0.5,0.25));
#9855=CARTESIAN_POINT('',(-0.5,0.5,0.25));
#9856=CARTESIAN_POINT('',(0.5,0.5,0.25));
#9857=CARTESIAN_POINT('',(0.5,0.5,0.25));
#9858=CARTESIAN_POINT('',(0.5,0.29,0.25));
#9859=CARTESIAN_POINT('Origin',(0.5,0.5,0.25));
#9860=CARTESIAN_POINT('',(-0.5,0.5,0.4));
#9861=CARTESIAN_POINT('',(-0.5,0.5,0.25));
#9862=CARTESIAN_POINT('',(0.5,0.5,0.4));
#9863=CARTESIAN_POINT('',(0.5,0.5,0.4));
#9864=CARTESIAN_POINT('',(0.5,0.5,0.25));
#9865=CARTESIAN_POINT('Origin',(0.,0.,0.4));
#9866=CARTESIAN_POINT('',(-0.5,-0.5,0.4));
#9867=CARTESIAN_POINT('',(-0.5,0.5,0.4));
#9868=CARTESIAN_POINT('',(0.5,-0.5,0.4));
#9869=CARTESIAN_POINT('',(-0.5,-0.5,0.4));
#9870=CARTESIAN_POINT('',(0.5,-0.3,0.4));
#9871=CARTESIAN_POINT('',(-0.2117,2.59257727379495E-17,0.4));
#9872=CARTESIAN_POINT('Origin',(0.,0.,0.4));
#9873=CARTESIAN_POINT('Origin',(-0.5,0.3,0.));
#9874=CARTESIAN_POINT('',(-0.5,0.3,0.15));
#9875=CARTESIAN_POINT('',(-0.5,0.3,0.));
#9876=CARTESIAN_POINT('',(-0.5,0.15,0.));
#9877=CARTESIAN_POINT('',(-0.5,0.225,0.075));
#9878=CARTESIAN_POINT('',(-0.5,-0.15,0.));
#9879=CARTESIAN_POINT('',(-0.5,0.3,0.));
#9880=CARTESIAN_POINT('',(-0.5,-0.3,0.15));
#9881=CARTESIAN_POINT('',(-0.5,-0.075,-0.075));
#9882=CARTESIAN_POINT('',(-0.5,-0.3,0.25));
#9883=CARTESIAN_POINT('',(-0.5,-0.3,0.));
#9884=CARTESIAN_POINT('',(-0.5,-0.5,0.25));
#9885=CARTESIAN_POINT('',(-0.5,-0.29,0.25));
#9886=CARTESIAN_POINT('',(-0.5,-0.5,0.25));
#9887=CARTESIAN_POINT('Origin',(-0.5,-0.5,0.25));
#9888=CARTESIAN_POINT('',(0.5,-0.5,0.25));
#9889=CARTESIAN_POINT('',(-0.5,-0.5,0.25));
#9890=CARTESIAN_POINT('',(0.5,-0.5,0.25));
#9891=CARTESIAN_POINT('Origin',(0.,-0.395,0.25));
#9892=CARTESIAN_POINT('',(0.5,-0.3,0.25));
#9893=CARTESIAN_POINT('',(-0.25,-0.3,0.25));
#9894=CARTESIAN_POINT('',(0.5,-0.5,0.25));
#9895=CARTESIAN_POINT('Origin',(0.5,-0.3,0.));
#9896=CARTESIAN_POINT('',(0.5,-0.3,0.15));
#9897=CARTESIAN_POINT('',(0.5,-0.3,0.));
#9898=CARTESIAN_POINT('',(0.5,-0.15,0.));
#9899=CARTESIAN_POINT('',(0.5,-0.225,0.075));
#9900=CARTESIAN_POINT('',(0.5,0.15,0.));
#9901=CARTESIAN_POINT('',(0.5,-0.3,0.));
#9902=CARTESIAN_POINT('',(0.5,0.3,0.15));
#9903=CARTESIAN_POINT('',(0.5,0.075,-0.075));
#9904=CARTESIAN_POINT('',(0.5,0.3,0.));
#9905=CARTESIAN_POINT('Origin',(-0.5,-0.3,0.));
#9906=CARTESIAN_POINT('',(-0.25,-0.3,0.15));
#9907=CARTESIAN_POINT('Origin',(-0.25,-0.225,0.075));
#9908=CARTESIAN_POINT('',(-0.149388386429468,-0.15,0.));
#9909=CARTESIAN_POINT('',(-0.25,-0.15,0.));
#9910=CARTESIAN_POINT('',(0.149388386429468,-0.15,0.));
#9911=CARTESIAN_POINT('Origin',(0.,0.,-0.15));
#9912=CARTESIAN_POINT('',(-0.25,-0.15,0.));
#9913=CARTESIAN_POINT('Origin',(0.,0.,-0.1));
#9914=CARTESIAN_POINT('',(-0.2117,-2.59257727379495E-17,0.));
#9915=CARTESIAN_POINT('Origin',(0.,0.,0.));
#9916=CARTESIAN_POINT('',(-0.2117,-2.59257727379495E-17,-0.1));
#9917=CARTESIAN_POINT('',(-0.149388386429468,0.15,0.));
#9918=CARTESIAN_POINT('Origin',(0.,0.,0.));
#9919=CARTESIAN_POINT('',(0.149388386429468,0.15,0.));
#9920=CARTESIAN_POINT('Origin',(0.,0.,-0.15));
#9921=CARTESIAN_POINT('Origin',(0.,0.,0.));
#9922=CARTESIAN_POINT('Origin',(0.,0.,0.));
#9923=CARTESIAN_POINT('',(0.25,0.15,0.));
#9924=CARTESIAN_POINT('Origin',(0.,0.,0.));
#9925=CARTESIAN_POINT('',(0.25,0.15,0.));
#9926=CARTESIAN_POINT('Origin',(0.25,0.225,0.075));
#9927=CARTESIAN_POINT('',(0.25,0.3,0.15));
#9928=CARTESIAN_POINT('Origin',(0.5,0.3,0.));
#9929=CARTESIAN_POINT('',(0.,0.,0.));
#9930=CARTESIAN_POINT('Origin',(0.,0.09,0.));
#9931=CARTESIAN_POINT('',(-0.285,0.1,3.49024337756996E-17));
#9932=CARTESIAN_POINT('Origin',(0.,0.1,0.));
#9933=CARTESIAN_POINT('',(-0.265,0.08,-3.24531401774049E-17));
#9934=CARTESIAN_POINT('',(-0.275,0.09,3.36777869765522E-17));
#9935=CARTESIAN_POINT('Origin',(0.,0.08,0.));
#9936=CARTESIAN_POINT('Origin',(0.,0.,0.));
#9937=CARTESIAN_POINT('',(-0.265,0.,3.24531401774049E-17));
#9938=CARTESIAN_POINT('',(-0.265,0.,3.24531401774049E-17));
#9939=CARTESIAN_POINT('Origin',(0.,0.,0.));
#9940=CARTESIAN_POINT('Origin',(0.,0.1,0.));
#9941=CARTESIAN_POINT('',(-0.5,0.1,6.12323399573677E-17));
#9942=CARTESIAN_POINT('Origin',(0.,0.1,0.));
#9943=CARTESIAN_POINT('Origin',(0.,0.,0.));
#9944=CARTESIAN_POINT('',(-0.5,0.,6.12323399573677E-17));
#9945=CARTESIAN_POINT('',(-0.5,0.,6.12323399573677E-17));
#9946=CARTESIAN_POINT('Origin',(0.,0.,0.));
#9947=CARTESIAN_POINT('Origin',(0.,0.,0.));
#9948=CARTESIAN_POINT('',(0.,0.,0.));
#9949=CARTESIAN_POINT('Origin',(5.,-18.,-0.5));
#9950=CARTESIAN_POINT('',(5.,-18.,-0.5));
#9951=CARTESIAN_POINT('',(-5.,-18.,-0.5));
#9952=CARTESIAN_POINT('',(5.,-18.,-0.5));
#9953=CARTESIAN_POINT('',(-5.,-18.,0.));
#9954=CARTESIAN_POINT('',(-5.,-18.,-0.5));
#9955=CARTESIAN_POINT('',(5.,-18.,0.));
#9956=CARTESIAN_POINT('',(5.,-18.,0.));
#9957=CARTESIAN_POINT('',(5.,-18.,-0.5));
#9958=CARTESIAN_POINT('Origin',(5.,-19.,-0.5));
#9959=CARTESIAN_POINT('',(5.,-19.,-0.5));
#9960=CARTESIAN_POINT('',(5.,-19.,-0.5));
#9961=CARTESIAN_POINT('',(5.,-19.,0.));
#9962=CARTESIAN_POINT('',(5.,-19.,0.));
#9963=CARTESIAN_POINT('',(5.,-19.,-0.5));
#9964=CARTESIAN_POINT('Origin',(-5.,-19.,-0.5));
#9965=CARTESIAN_POINT('',(-5.,-19.,-0.5));
#9966=CARTESIAN_POINT('',(-5.,-19.,-0.5));
#9967=CARTESIAN_POINT('',(-5.,-19.,0.));
#9968=CARTESIAN_POINT('',(-5.,-19.,0.));
#9969=CARTESIAN_POINT('',(-5.,-19.,-0.5));
#9970=CARTESIAN_POINT('Origin',(-5.,-18.,-0.5));
#9971=CARTESIAN_POINT('',(-5.,-18.,-0.5));
#9972=CARTESIAN_POINT('',(-5.,-18.,0.));
#9973=CARTESIAN_POINT('Origin',(0.,-18.5,0.));
#9974=CARTESIAN_POINT('Origin',(0.,-18.5,-0.5));
#9975=CARTESIAN_POINT('',(0.,0.,0.));
#9976=CARTESIAN_POINT('Origin',(5.,19.,-0.5));
#9977=CARTESIAN_POINT('',(5.,19.,-0.5));
#9978=CARTESIAN_POINT('',(-5.,19.,-0.5));
#9979=CARTESIAN_POINT('',(5.,19.,-0.5));
#9980=CARTESIAN_POINT('',(-5.,19.,0.));
#9981=CARTESIAN_POINT('',(-5.,19.,-0.5));
#9982=CARTESIAN_POINT('',(5.,19.,0.));
#9983=CARTESIAN_POINT('',(5.,19.,0.));
#9984=CARTESIAN_POINT('',(5.,19.,-0.5));
#9985=CARTESIAN_POINT('Origin',(5.,18.,-0.5));
#9986=CARTESIAN_POINT('',(5.,18.,-0.5));
#9987=CARTESIAN_POINT('',(5.,18.,-0.5));
#9988=CARTESIAN_POINT('',(5.,18.,0.));
#9989=CARTESIAN_POINT('',(5.,18.,0.));
#9990=CARTESIAN_POINT('',(5.,18.,-0.5));
#9991=CARTESIAN_POINT('Origin',(-5.,18.,-0.5));
#9992=CARTESIAN_POINT('',(-5.,18.,-0.5));
#9993=CARTESIAN_POINT('',(-5.,18.,-0.5));
#9994=CARTESIAN_POINT('',(-5.,18.,0.));
#9995=CARTESIAN_POINT('',(-5.,18.,0.));
#9996=CARTESIAN_POINT('',(-5.,18.,-0.5));
#9997=CARTESIAN_POINT('Origin',(-5.,19.,-0.5));
#9998=CARTESIAN_POINT('',(-5.,19.,-0.5));
#9999=CARTESIAN_POINT('',(-5.,19.,0.));
#10000=CARTESIAN_POINT('Origin',(0.,18.5,0.));
#10001=CARTESIAN_POINT('Origin',(0.,18.5,-0.5));
#10002=CARTESIAN_POINT('',(0.,0.,0.));
#10003=CARTESIAN_POINT('Origin',(-3.5,-12.5,2.7));
#10004=CARTESIAN_POINT('',(-3.83,-12.5,2.8));
#10005=CARTESIAN_POINT('Origin',(-3.5,-12.5,2.8));
#10006=CARTESIAN_POINT('',(-3.83,-12.5,3.8));
#10007=CARTESIAN_POINT('',(-3.83,-12.5,2.7));
#10008=CARTESIAN_POINT('Origin',(-3.5,-12.5,3.8));
#10009=CARTESIAN_POINT('Origin',(3.5,-12.5,2.7));
#10010=CARTESIAN_POINT('',(3.17,-12.5,2.8));
#10011=CARTESIAN_POINT('Origin',(3.5,-12.5,2.8));
#10012=CARTESIAN_POINT('',(3.17,-12.5,3.8));
#10013=CARTESIAN_POINT('',(3.17,-12.5,2.7));
#10014=CARTESIAN_POINT('Origin',(3.5,-12.5,3.8));
#10015=CARTESIAN_POINT('Origin',(0.,-11.6,6.95959179422654));
#10016=CARTESIAN_POINT('',(1.03956420750473,-11.5,6.6));
#10017=CARTESIAN_POINT('',(-1.03956420750473,-11.5,6.6));
#10018=CARTESIAN_POINT('Origin',(0.,-11.5,6.95959179422654));
#10019=CARTESIAN_POINT('',(1.03956420750473,-10.8,6.6));
#10020=CARTESIAN_POINT('',(1.03956420750473,-11.6,6.6));
#10021=CARTESIAN_POINT('',(-1.03956420750473,-10.8,6.6));
#10022=CARTESIAN_POINT('Origin',(0.,-10.8,6.95959179422654));
#10023=CARTESIAN_POINT('',(-1.03956420750473,-11.6,6.6));
#10024=CARTESIAN_POINT('Origin',(4.8,-10.8,2.8));
#10025=CARTESIAN_POINT('',(4.8,-10.8,6.6));
#10026=CARTESIAN_POINT('',(4.8,-10.8,6.6));
#10027=CARTESIAN_POINT('',(4.8,-10.8,2.8));
#10028=CARTESIAN_POINT('',(4.8,-10.8,2.8));
#10029=CARTESIAN_POINT('',(-4.8,-10.8,2.8));
#10030=CARTESIAN_POINT('',(4.8,-10.8,2.8));
#10031=CARTESIAN_POINT('',(-4.8,-10.8,6.6));
#10032=CARTESIAN_POINT('',(-4.8,-10.8,2.8));
#10033=CARTESIAN_POINT('',(4.8,-10.8,6.6));
#10034=CARTESIAN_POINT('',(1.5,-10.8,5.));
#10035=CARTESIAN_POINT('Origin',(2.,-10.8,5.));
#10036=CARTESIAN_POINT('',(-2.5,-10.8,5.));
#10037=CARTESIAN_POINT('Origin',(-2.,-10.8,5.));
#10038=CARTESIAN_POINT('Origin',(0.,-11.15,6.6));
#10039=CARTESIAN_POINT('',(4.8,-11.5,6.6));
#10040=CARTESIAN_POINT('',(-4.8,-11.5,6.6));
#10041=CARTESIAN_POINT('',(4.8,-11.5,6.6));
#10042=CARTESIAN_POINT('Origin',(-2.,-11.6,5.));
#10043=CARTESIAN_POINT('',(-2.5,-11.5,5.));
#10044=CARTESIAN_POINT('Origin',(-2.,-11.5,5.));
#10045=CARTESIAN_POINT('',(-2.5,-11.6,5.));
#10046=CARTESIAN_POINT('Origin',(2.,-11.6,5.));
#10047=CARTESIAN_POINT('',(1.5,-11.5,5.));
#10048=CARTESIAN_POINT('Origin',(2.,-11.5,5.));
#10049=CARTESIAN_POINT('',(1.5,-11.6,5.));
#10050=CARTESIAN_POINT('Origin',(-4.8,-13.5,3.8));
#10051=CARTESIAN_POINT('',(4.8,-13.5,3.8));
#10052=CARTESIAN_POINT('',(-4.8,-13.5,3.8));
#10053=CARTESIAN_POINT('',(4.8,-13.5,3.8));
#10054=CARTESIAN_POINT('',(4.8,-11.5,3.8));
#10055=CARTESIAN_POINT('',(4.8,-13.5,3.8));
#10056=CARTESIAN_POINT('',(-4.8,-11.5,3.8));
#10057=CARTESIAN_POINT('',(-4.8,-11.5,3.8));
#10058=CARTESIAN_POINT('',(-4.8,-13.5,3.8));
#10059=CARTESIAN_POINT('Origin',(0.,-13.5,3.3));
#10060=CARTESIAN_POINT('',(-4.8,-13.5,2.8));
#10061=CARTESIAN_POINT('',(-4.8,-13.5,3.8));
#10062=CARTESIAN_POINT('',(4.8,-13.5,2.8));
#10063=CARTESIAN_POINT('',(-4.8,-13.5,2.8));
#10064=CARTESIAN_POINT('',(4.8,-13.5,2.8));
#10065=CARTESIAN_POINT('Origin',(4.8,-11.5,2.8));
#10066=CARTESIAN_POINT('',(4.8,-13.5,2.8));
#10067=CARTESIAN_POINT('',(4.8,-11.5,2.8));
#10068=CARTESIAN_POINT('Origin',(-4.8,-11.5,2.8));
#10069=CARTESIAN_POINT('',(-4.8,-11.5,6.6));
#10070=CARTESIAN_POINT('',(-4.8,-11.5,6.6));
#10071=CARTESIAN_POINT('',(-4.8,-11.5,2.8));
#10072=CARTESIAN_POINT('Origin',(-4.8,-10.8,2.8));
#10073=CARTESIAN_POINT('',(-4.8,-10.8,2.8));
#10074=CARTESIAN_POINT('',(-4.8,-10.8,6.6));
#10075=CARTESIAN_POINT('Origin',(0.,-11.15,6.6));
#10076=CARTESIAN_POINT('Origin',(0.,-11.15,2.8));
#10077=CARTESIAN_POINT('',(0.,0.,0.));
#10078=CARTESIAN_POINT('Origin',(-2.,-10.4,5.));
#10079=CARTESIAN_POINT('',(-2.165,-10.4,5.));
#10080=CARTESIAN_POINT('Origin',(-2.,-10.4,5.));
#10081=CARTESIAN_POINT('',(-2.165,-9.2,5.));
#10082=CARTESIAN_POINT('',(-2.165,-10.4,5.));
#10083=CARTESIAN_POINT('Origin',(-2.,-9.2,5.));
#10084=CARTESIAN_POINT('Origin',(-2.,-10.4,5.));
#10085=CARTESIAN_POINT('Origin',(-2.,-11.5,5.));
#10086=CARTESIAN_POINT('',(-2.8,-11.5,5.));
#10087=CARTESIAN_POINT('Origin',(-2.,-11.5,5.));
#10088=CARTESIAN_POINT('',(-2.5,-11.5,5.));
#10089=CARTESIAN_POINT('Origin',(-2.,-11.5,5.));
#10090=CARTESIAN_POINT('Origin',(-2.,-11.8,5.));
#10091=CARTESIAN_POINT('',(-2.8,-11.8,5.));
#10092=CARTESIAN_POINT('',(-2.8,-11.8,5.));
#10093=CARTESIAN_POINT('Origin',(-2.,-11.8,5.));
#10094=CARTESIAN_POINT('Origin',(-2.,-11.8,5.));
#10095=CARTESIAN_POINT('Origin',(-2.,-11.5,5.));
#10096=CARTESIAN_POINT('',(-2.5,-9.2,5.));
#10097=CARTESIAN_POINT('Origin',(-2.,-9.2,5.));
#10098=CARTESIAN_POINT('',(-2.5,-11.5,5.));
#10099=CARTESIAN_POINT('Origin',(-2.,-9.2,5.));
#10100=CARTESIAN_POINT('',(0.,0.,0.));
#10101=CARTESIAN_POINT('Origin',(-2.,-10.8,5.));
#10102=CARTESIAN_POINT('',(-2.505,-10.45,5.));
#10103=CARTESIAN_POINT('Origin',(-2.,-10.45,5.));
#10104=CARTESIAN_POINT('',(-2.505,-10.8,5.));
#10105=CARTESIAN_POINT('',(-2.505,-10.8,5.));
#10106=CARTESIAN_POINT('Origin',(-2.,-10.8,5.));
#10107=CARTESIAN_POINT('Origin',(-2.,-10.8,5.));
#10108=CARTESIAN_POINT('',(-2.7,-10.45,5.));
#10109=CARTESIAN_POINT('Origin',(-2.,-10.45,5.));
#10110=CARTESIAN_POINT('',(-2.7,-10.8,5.));
#10111=CARTESIAN_POINT('',(-2.7,-10.8,5.));
#10112=CARTESIAN_POINT('Origin',(-2.,-10.8,5.));
#10113=CARTESIAN_POINT('Origin',(-2.,-10.45,5.));
#10114=CARTESIAN_POINT('Origin',(-2.,-10.8,5.));
#10115=CARTESIAN_POINT('',(0.,0.,0.));
#10116=CARTESIAN_POINT('Origin',(-2.,-9.55,5.));
#10117=CARTESIAN_POINT('',(-2.505,-9.2,5.));
#10118=CARTESIAN_POINT('Origin',(-2.,-9.2,5.));
#10119=CARTESIAN_POINT('',(-2.505,-9.55,5.));
#10120=CARTESIAN_POINT('',(-2.505,-9.55,5.));
#10121=CARTESIAN_POINT('Origin',(-2.,-9.55,5.));
#10122=CARTESIAN_POINT('Origin',(-2.,-9.55,5.));
#10123=CARTESIAN_POINT('',(-2.7,-9.2,5.));
#10124=CARTESIAN_POINT('Origin',(-2.,-9.2,5.));
#10125=CARTESIAN_POINT('',(-2.7,-9.55,5.));
#10126=CARTESIAN_POINT('',(-2.7,-9.55,5.));
#10127=CARTESIAN_POINT('Origin',(-2.,-9.55,5.));
#10128=CARTESIAN_POINT('Origin',(-2.,-9.2,5.));
#10129=CARTESIAN_POINT('Origin',(-2.,-9.55,5.));
#10130=CARTESIAN_POINT('',(0.,0.,0.));
#10131=CARTESIAN_POINT('Origin',(-2.,-9.2,5.));
#10132=CARTESIAN_POINT('',(-2.225,-9.,5.));
#10133=CARTESIAN_POINT('Origin',(-2.,-9.,5.));
#10134=CARTESIAN_POINT('',(-2.225,-9.2,5.));
#10135=CARTESIAN_POINT('',(-2.225,-9.2,5.));
#10136=CARTESIAN_POINT('Origin',(-2.,-9.2,5.));
#10137=CARTESIAN_POINT('Origin',(-2.,-9.2,5.));
#10138=CARTESIAN_POINT('',(-2.8,-9.,5.));
#10139=CARTESIAN_POINT('Origin',(-2.,-9.,5.));
#10140=CARTESIAN_POINT('',(-2.8,-9.2,5.));
#10141=CARTESIAN_POINT('',(-2.8,-9.2,5.));
#10142=CARTESIAN_POINT('Origin',(-2.,-9.2,5.));
#10143=CARTESIAN_POINT('Origin',(-2.,-9.,5.));
#10144=CARTESIAN_POINT('Origin',(-2.,-9.2,5.));
#10145=CARTESIAN_POINT('',(0.,0.,0.));
#10146=CARTESIAN_POINT('Origin',(2.,-10.4,5.));
#10147=CARTESIAN_POINT('',(1.835,-10.4,5.));
#10148=CARTESIAN_POINT('Origin',(2.,-10.4,5.));
#10149=CARTESIAN_POINT('',(1.835,-9.2,5.));
#10150=CARTESIAN_POINT('',(1.835,-10.4,5.));
#10151=CARTESIAN_POINT('Origin',(2.,-9.2,5.));
#10152=CARTESIAN_POINT('Origin',(2.,-10.4,5.));
#10153=CARTESIAN_POINT('Origin',(2.,-11.5,5.));
#10154=CARTESIAN_POINT('',(1.2,-11.5,5.));
#10155=CARTESIAN_POINT('Origin',(2.,-11.5,5.));
#10156=CARTESIAN_POINT('',(1.5,-11.5,5.));
#10157=CARTESIAN_POINT('Origin',(2.,-11.5,5.));
#10158=CARTESIAN_POINT('Origin',(2.,-11.8,5.));
#10159=CARTESIAN_POINT('',(1.2,-11.8,5.));
#10160=CARTESIAN_POINT('',(1.2,-11.8,5.));
#10161=CARTESIAN_POINT('Origin',(2.,-11.8,5.));
#10162=CARTESIAN_POINT('Origin',(2.,-11.8,5.));
#10163=CARTESIAN_POINT('Origin',(2.,-11.5,5.));
#10164=CARTESIAN_POINT('',(1.5,-9.2,5.));
#10165=CARTESIAN_POINT('Origin',(2.,-9.2,5.));
#10166=CARTESIAN_POINT('',(1.5,-11.5,5.));
#10167=CARTESIAN_POINT('Origin',(2.,-9.2,5.));
#10168=CARTESIAN_POINT('',(0.,0.,0.));
#10169=CARTESIAN_POINT('Origin',(2.,-9.55,5.));
#10170=CARTESIAN_POINT('',(1.495,-9.2,5.));
#10171=CARTESIAN_POINT('Origin',(2.,-9.2,5.));
#10172=CARTESIAN_POINT('',(1.495,-9.55,5.));
#10173=CARTESIAN_POINT('',(1.495,-9.55,5.));
#10174=CARTESIAN_POINT('Origin',(2.,-9.55,5.));
#10175=CARTESIAN_POINT('Origin',(2.,-9.55,5.));
#10176=CARTESIAN_POINT('',(1.3,-9.2,5.));
#10177=CARTESIAN_POINT('Origin',(2.,-9.2,5.));
#10178=CARTESIAN_POINT('',(1.3,-9.55,5.));
#10179=CARTESIAN_POINT('',(1.3,-9.55,5.));
#10180=CARTESIAN_POINT('Origin',(2.,-9.55,5.));
#10181=CARTESIAN_POINT('Origin',(2.,-9.2,5.));
#10182=CARTESIAN_POINT('Origin',(2.,-9.55,5.));
#10183=CARTESIAN_POINT('',(0.,0.,0.));
#10184=CARTESIAN_POINT('Origin',(2.,-9.2,5.));
#10185=CARTESIAN_POINT('',(1.775,-9.,5.));
#10186=CARTESIAN_POINT('Origin',(2.,-9.,5.));
#10187=CARTESIAN_POINT('',(1.775,-9.2,5.));
#10188=CARTESIAN_POINT('',(1.775,-9.2,5.));
#10189=CARTESIAN_POINT('Origin',(2.,-9.2,5.));
#10190=CARTESIAN_POINT('Origin',(2.,-9.2,5.));
#10191=CARTESIAN_POINT('',(1.2,-9.,5.));
#10192=CARTESIAN_POINT('Origin',(2.,-9.,5.));
#10193=CARTESIAN_POINT('',(1.2,-9.2,5.));
#10194=CARTESIAN_POINT('',(1.2,-9.2,5.));
#10195=CARTESIAN_POINT('Origin',(2.,-9.2,5.));
#10196=CARTESIAN_POINT('Origin',(2.,-9.,5.));
#10197=CARTESIAN_POINT('Origin',(2.,-9.2,5.));
#10198=CARTESIAN_POINT('',(0.,0.,0.));
#10199=CARTESIAN_POINT('Origin',(-3.5,7.5,2.7));
#10200=CARTESIAN_POINT('',(-3.83,7.5,2.8));
#10201=CARTESIAN_POINT('Origin',(-3.5,7.5,2.8));
#10202=CARTESIAN_POINT('',(-3.83,7.5,3.8));
#10203=CARTESIAN_POINT('',(-3.83,7.5,2.7));
#10204=CARTESIAN_POINT('Origin',(-3.5,7.5,3.8));
#10205=CARTESIAN_POINT('Origin',(3.5,7.5,2.7));
#10206=CARTESIAN_POINT('',(3.17,7.5,2.8));
#10207=CARTESIAN_POINT('Origin',(3.5,7.5,2.8));
#10208=CARTESIAN_POINT('',(3.17,7.5,3.8));
#10209=CARTESIAN_POINT('',(3.17,7.5,2.7));
#10210=CARTESIAN_POINT('Origin',(3.5,7.5,3.8));
#10211=CARTESIAN_POINT('Origin',(0.,8.4,6.95959179422654));
#10212=CARTESIAN_POINT('',(1.03956420750473,8.5,6.6));
#10213=CARTESIAN_POINT('',(-1.03956420750473,8.5,6.6));
#10214=CARTESIAN_POINT('Origin',(0.,8.5,6.95959179422654));
#10215=CARTESIAN_POINT('',(1.03956420750473,9.2,6.6));
#10216=CARTESIAN_POINT('',(1.03956420750473,8.4,6.6));
#10217=CARTESIAN_POINT('',(-1.03956420750473,9.2,6.6));
#10218=CARTESIAN_POINT('Origin',(0.,9.2,6.95959179422654));
#10219=CARTESIAN_POINT('',(-1.03956420750473,8.4,6.6));
#10220=CARTESIAN_POINT('Origin',(4.8,9.2,2.8));
#10221=CARTESIAN_POINT('',(4.8,9.2,6.6));
#10222=CARTESIAN_POINT('',(4.8,9.2,6.6));
#10223=CARTESIAN_POINT('',(4.8,9.2,2.8));
#10224=CARTESIAN_POINT('',(4.8,9.2,2.8));
#10225=CARTESIAN_POINT('',(-4.8,9.2,2.8));
#10226=CARTESIAN_POINT('',(4.8,9.2,2.8));
#10227=CARTESIAN_POINT('',(-4.8,9.2,6.6));
#10228=CARTESIAN_POINT('',(-4.8,9.2,2.8));
#10229=CARTESIAN_POINT('',(4.8,9.2,6.6));
#10230=CARTESIAN_POINT('',(1.5,9.2,5.));
#10231=CARTESIAN_POINT('Origin',(2.,9.2,5.));
#10232=CARTESIAN_POINT('',(-2.5,9.2,5.));
#10233=CARTESIAN_POINT('Origin',(-2.,9.2,5.));
#10234=CARTESIAN_POINT('Origin',(0.,8.85,6.6));
#10235=CARTESIAN_POINT('',(4.8,8.5,6.6));
#10236=CARTESIAN_POINT('',(-4.8,8.5,6.6));
#10237=CARTESIAN_POINT('',(4.8,8.5,6.6));
#10238=CARTESIAN_POINT('Origin',(-2.,8.4,5.));
#10239=CARTESIAN_POINT('',(-2.5,8.5,5.));
#10240=CARTESIAN_POINT('Origin',(-2.,8.5,5.));
#10241=CARTESIAN_POINT('',(-2.5,8.4,5.));
#10242=CARTESIAN_POINT('Origin',(2.,8.4,5.));
#10243=CARTESIAN_POINT('',(1.5,8.5,5.));
#10244=CARTESIAN_POINT('Origin',(2.,8.5,5.));
#10245=CARTESIAN_POINT('',(1.5,8.4,5.));
#10246=CARTESIAN_POINT('Origin',(-4.8,6.5,3.8));
#10247=CARTESIAN_POINT('',(4.8,6.5,3.8));
#10248=CARTESIAN_POINT('',(-4.8,6.5,3.8));
#10249=CARTESIAN_POINT('',(4.8,6.5,3.8));
#10250=CARTESIAN_POINT('',(4.8,8.5,3.8));
#10251=CARTESIAN_POINT('',(4.8,6.5,3.8));
#10252=CARTESIAN_POINT('',(-4.8,8.5,3.8));
#10253=CARTESIAN_POINT('',(-4.8,8.5,3.8));
#10254=CARTESIAN_POINT('',(-4.8,6.5,3.8));
#10255=CARTESIAN_POINT('Origin',(0.,6.5,3.3));
#10256=CARTESIAN_POINT('',(-4.8,6.5,2.8));
#10257=CARTESIAN_POINT('',(-4.8,6.5,3.8));
#10258=CARTESIAN_POINT('',(4.8,6.5,2.8));
#10259=CARTESIAN_POINT('',(-4.8,6.5,2.8));
#10260=CARTESIAN_POINT('',(4.8,6.5,2.8));
#10261=CARTESIAN_POINT('Origin',(4.8,8.5,2.8));
#10262=CARTESIAN_POINT('',(4.8,6.5,2.8));
#10263=CARTESIAN_POINT('',(4.8,8.5,2.8));
#10264=CARTESIAN_POINT('Origin',(-4.8,8.5,2.8));
#10265=CARTESIAN_POINT('',(-4.8,8.5,6.6));
#10266=CARTESIAN_POINT('',(-4.8,8.5,6.6));
#10267=CARTESIAN_POINT('',(-4.8,8.5,2.8));
#10268=CARTESIAN_POINT('Origin',(-4.8,9.2,2.8));
#10269=CARTESIAN_POINT('',(-4.8,9.2,2.8));
#10270=CARTESIAN_POINT('',(-4.8,9.2,6.6));
#10271=CARTESIAN_POINT('Origin',(0.,8.85,6.6));
#10272=CARTESIAN_POINT('Origin',(0.,8.85,2.8));
#10273=CARTESIAN_POINT('',(0.,0.,0.));
#10274=CARTESIAN_POINT('Origin',(0.144337567297406,-0.6,-0.25));
#10275=CARTESIAN_POINT('',(0.288675134594813,-0.6,0.));
#10276=CARTESIAN_POINT('',(0.144337567297406,-0.6,-0.25));
#10277=CARTESIAN_POINT('',(0.288675134594813,-0.6,0.));
#10278=CARTESIAN_POINT('',(0.144337567297406,-0.96,-0.25));
#10279=CARTESIAN_POINT('',(0.144337567297406,-0.6,-0.25));
#10280=CARTESIAN_POINT('',(0.288675134594813,-0.96,0.));
#10281=CARTESIAN_POINT('',(0.288675134594813,-0.96,0.));
#10282=CARTESIAN_POINT('',(0.288675134594813,-0.6,0.));
#10283=CARTESIAN_POINT('Origin',(-0.144337567297406,-0.6,-0.25));
#10284=CARTESIAN_POINT('',(-0.144337567297406,-0.6,-0.25));
#10285=CARTESIAN_POINT('',(0.144337567297406,-0.6,-0.25));
#10286=CARTESIAN_POINT('',(-0.144337567297406,-0.96,-0.25));
#10287=CARTESIAN_POINT('',(-0.144337567297406,-0.6,-0.25));
#10288=CARTESIAN_POINT('',(0.144337567297406,-0.96,-0.25));
#10289=CARTESIAN_POINT('Origin',(-0.288675134594813,-0.6,-8.32667268468867E-17));
#10290=CARTESIAN_POINT('',(-0.288675134594813,-0.6,-3.53525079574969E-17));
#10291=CARTESIAN_POINT('',(-0.144337567297406,-0.6,-0.25));
#10292=CARTESIAN_POINT('',(-0.288675134594813,-0.96,-5.55111512312578E-17));
#10293=CARTESIAN_POINT('',(-0.288675134594813,-0.6,-3.53525079574969E-17));
#10294=CARTESIAN_POINT('',(-0.144337567297406,-0.96,-0.25));
#10295=CARTESIAN_POINT('Origin',(-0.144337567297407,-0.6,0.25));
#10296=CARTESIAN_POINT('',(-0.144337567297407,-0.6,0.25));
#10297=CARTESIAN_POINT('',(-0.288675134594813,-0.6,-3.53525079574969E-17));
#10298=CARTESIAN_POINT('',(-0.144337567297407,-0.96,0.25));
#10299=CARTESIAN_POINT('',(-0.144337567297407,-0.6,0.25));
#10300=CARTESIAN_POINT('',(-0.288675134594813,-0.96,-3.53525079574969E-17));
#10301=CARTESIAN_POINT('Origin',(0.144337567297406,-0.6,0.25));
#10302=CARTESIAN_POINT('',(0.144337567297406,-0.6,0.25));
#10303=CARTESIAN_POINT('',(-0.144337567297407,-0.6,0.25));
#10304=CARTESIAN_POINT('',(0.144337567297406,-0.96,0.25));
#10305=CARTESIAN_POINT('',(0.144337567297406,-0.6,0.25));
#10306=CARTESIAN_POINT('',(-0.144337567297407,-0.96,0.25));
#10307=CARTESIAN_POINT('Origin',(0.288675134594813,-0.6,0.));
#10308=CARTESIAN_POINT('',(0.144337567297406,-0.6,0.25));
#10309=CARTESIAN_POINT('',(0.144337567297406,-0.96,0.25));
#10310=CARTESIAN_POINT('Origin',(0.,-0.6,0.));
#10311=CARTESIAN_POINT('Origin',(0.,-0.96,0.));
#10312=CARTESIAN_POINT('Origin',(0.,-1.8,0.));
#10313=CARTESIAN_POINT('',(-0.2942,-1.8,3.60291088309151E-17));
#10314=CARTESIAN_POINT('Origin',(0.,-1.8,0.));
#10315=CARTESIAN_POINT('Origin',(0.45,0.6,0.));
#10316=CARTESIAN_POINT('',(-0.45,0.6,-5.51091059616309E-17));
#10317=CARTESIAN_POINT('Origin',(0.,0.6,0.));
#10318=CARTESIAN_POINT('Origin',(0.,0.575,0.));
#10319=CARTESIAN_POINT('',(-0.5,0.55,-6.12323399573677E-17));
#10320=CARTESIAN_POINT('Origin',(0.,0.55,0.));
#10321=CARTESIAN_POINT('',(-0.475,0.575,-5.81707229594993E-17));
#10322=CARTESIAN_POINT('Origin',(0.,0.29,0.));
#10323=CARTESIAN_POINT('',(-0.5,0.0299999999999998,-6.12323399573677E-17));
#10324=CARTESIAN_POINT('Origin',(0.,0.0299999999999998,0.));
#10325=CARTESIAN_POINT('',(-0.5,0.29,-6.12323399573677E-17));
#10326=CARTESIAN_POINT('Origin',(0.,0.0150000000000001,0.));
#10327=CARTESIAN_POINT('',(-0.47,7.11236625150491E-17,-5.75583995599256E-17));
#10328=CARTESIAN_POINT('Origin',(0.,0.,0.));
#10329=CARTESIAN_POINT('',(-0.485,0.0150000000000001,-5.93953697586466E-17));
#10330=CARTESIAN_POINT('Origin',(0.32,0.,0.));
#10331=CARTESIAN_POINT('',(-0.32,-6.93889390390723E-18,-3.91886975727153E-17));
#10332=CARTESIAN_POINT('Origin',(0.,0.,0.));
#10333=CARTESIAN_POINT('Origin',(0.,-0.02,0.));
#10334=CARTESIAN_POINT('',(-0.2942,-0.0515999999999999,3.60291088309151E-17));
#10335=CARTESIAN_POINT('Origin',(0.,-0.0515999999999999,0.));
#10336=CARTESIAN_POINT('',(-0.31,-0.02,-3.7964050773568E-17));
#10337=CARTESIAN_POINT('Origin',(0.,-1.24,0.));
#10338=CARTESIAN_POINT('',(-0.2942,-1.24,-3.60291088309151E-17));
#10339=CARTESIAN_POINT('',(0.,0.,0.));
#10340=CARTESIAN_POINT('Origin',(-2.,9.6,5.));
#10341=CARTESIAN_POINT('',(-2.165,9.6,5.));
#10342=CARTESIAN_POINT('Origin',(-2.,9.6,5.));
#10343=CARTESIAN_POINT('',(-2.165,10.8,5.));
#10344=CARTESIAN_POINT('',(-2.165,9.6,5.));
#10345=CARTESIAN_POINT('Origin',(-2.,10.8,5.));
#10346=CARTESIAN_POINT('Origin',(-2.,9.6,5.));
#10347=CARTESIAN_POINT('Origin',(-2.,8.5,5.));
#10348=CARTESIAN_POINT('',(-2.8,8.5,5.));
#10349=CARTESIAN_POINT('Origin',(-2.,8.5,5.));
#10350=CARTESIAN_POINT('',(-2.5,8.5,5.));
#10351=CARTESIAN_POINT('Origin',(-2.,8.5,5.));
#10352=CARTESIAN_POINT('Origin',(-2.,8.2,5.));
#10353=CARTESIAN_POINT('',(-2.8,8.2,5.));
#10354=CARTESIAN_POINT('',(-2.8,8.2,5.));
#10355=CARTESIAN_POINT('Origin',(-2.,8.2,5.));
#10356=CARTESIAN_POINT('Origin',(-2.,8.2,5.));
#10357=CARTESIAN_POINT('Origin',(-2.,8.5,5.));
#10358=CARTESIAN_POINT('',(-2.5,10.8,5.));
#10359=CARTESIAN_POINT('Origin',(-2.,10.8,5.));
#10360=CARTESIAN_POINT('',(-2.5,8.5,5.));
#10361=CARTESIAN_POINT('Origin',(-2.,10.8,5.));
#10362=CARTESIAN_POINT('',(0.,0.,0.));
#10363=CARTESIAN_POINT('Origin',(-2.,10.45,5.));
#10364=CARTESIAN_POINT('',(-2.505,10.8,5.));
#10365=CARTESIAN_POINT('Origin',(-2.,10.8,5.));
#10366=CARTESIAN_POINT('',(-2.505,10.45,5.));
#10367=CARTESIAN_POINT('',(-2.505,10.45,5.));
#10368=CARTESIAN_POINT('Origin',(-2.,10.45,5.));
#10369=CARTESIAN_POINT('Origin',(-2.,10.45,5.));
#10370=CARTESIAN_POINT('',(-2.7,10.8,5.));
#10371=CARTESIAN_POINT('Origin',(-2.,10.8,5.));
#10372=CARTESIAN_POINT('',(-2.7,10.45,5.));
#10373=CARTESIAN_POINT('',(-2.7,10.45,5.));
#10374=CARTESIAN_POINT('Origin',(-2.,10.45,5.));
#10375=CARTESIAN_POINT('Origin',(-2.,10.8,5.));
#10376=CARTESIAN_POINT('Origin',(-2.,10.45,5.));
#10377=CARTESIAN_POINT('',(0.,0.,0.));
#10378=CARTESIAN_POINT('Origin',(-2.,10.8,5.));
#10379=CARTESIAN_POINT('',(-2.225,11.,5.));
#10380=CARTESIAN_POINT('Origin',(-2.,11.,5.));
#10381=CARTESIAN_POINT('',(-2.225,10.8,5.));
#10382=CARTESIAN_POINT('',(-2.225,10.8,5.));
#10383=CARTESIAN_POINT('Origin',(-2.,10.8,5.));
#10384=CARTESIAN_POINT('Origin',(-2.,10.8,5.));
#10385=CARTESIAN_POINT('',(-2.8,11.,5.));
#10386=CARTESIAN_POINT('Origin',(-2.,11.,5.));
#10387=CARTESIAN_POINT('',(-2.8,10.8,5.));
#10388=CARTESIAN_POINT('',(-2.8,10.8,5.));
#10389=CARTESIAN_POINT('Origin',(-2.,10.8,5.));
#10390=CARTESIAN_POINT('Origin',(-2.,11.,5.));
#10391=CARTESIAN_POINT('Origin',(-2.,10.8,5.));
#10392=CARTESIAN_POINT('',(0.,0.,0.));
#10393=CARTESIAN_POINT('Origin',(2.,9.6,5.));
#10394=CARTESIAN_POINT('',(1.835,9.6,5.));
#10395=CARTESIAN_POINT('Origin',(2.,9.6,5.));
#10396=CARTESIAN_POINT('',(1.835,10.8,5.));
#10397=CARTESIAN_POINT('',(1.835,9.6,5.));
#10398=CARTESIAN_POINT('Origin',(2.,10.8,5.));
#10399=CARTESIAN_POINT('Origin',(2.,9.6,5.));
#10400=CARTESIAN_POINT('Origin',(2.,8.5,5.));
#10401=CARTESIAN_POINT('',(1.2,8.5,5.));
#10402=CARTESIAN_POINT('Origin',(2.,8.5,5.));
#10403=CARTESIAN_POINT('',(1.5,8.5,5.));
#10404=CARTESIAN_POINT('Origin',(2.,8.5,5.));
#10405=CARTESIAN_POINT('Origin',(2.,8.2,5.));
#10406=CARTESIAN_POINT('',(1.2,8.2,5.));
#10407=CARTESIAN_POINT('',(1.2,8.2,5.));
#10408=CARTESIAN_POINT('Origin',(2.,8.2,5.));
#10409=CARTESIAN_POINT('Origin',(2.,8.2,5.));
#10410=CARTESIAN_POINT('Origin',(2.,8.5,5.));
#10411=CARTESIAN_POINT('',(1.5,10.8,5.));
#10412=CARTESIAN_POINT('Origin',(2.,10.8,5.));
#10413=CARTESIAN_POINT('',(1.5,8.5,5.));
#10414=CARTESIAN_POINT('Origin',(2.,10.8,5.));
#10415=CARTESIAN_POINT('',(0.,0.,0.));
#10416=CARTESIAN_POINT('Origin',(2.,10.45,5.));
#10417=CARTESIAN_POINT('',(1.495,10.8,5.));
#10418=CARTESIAN_POINT('Origin',(2.,10.8,5.));
#10419=CARTESIAN_POINT('',(1.495,10.45,5.));
#10420=CARTESIAN_POINT('',(1.495,10.45,5.));
#10421=CARTESIAN_POINT('Origin',(2.,10.45,5.));
#10422=CARTESIAN_POINT('Origin',(2.,10.45,5.));
#10423=CARTESIAN_POINT('',(1.3,10.8,5.));
#10424=CARTESIAN_POINT('Origin',(2.,10.8,5.));
#10425=CARTESIAN_POINT('',(1.3,10.45,5.));
#10426=CARTESIAN_POINT('',(1.3,10.45,5.));
#10427=CARTESIAN_POINT('Origin',(2.,10.45,5.));
#10428=CARTESIAN_POINT('Origin',(2.,10.8,5.));
#10429=CARTESIAN_POINT('Origin',(2.,10.45,5.));
#10430=CARTESIAN_POINT('',(0.,0.,0.));
#10431=CARTESIAN_POINT('Origin',(2.,10.8,5.));
#10432=CARTESIAN_POINT('',(1.775,11.,5.));
#10433=CARTESIAN_POINT('Origin',(2.,11.,5.));
#10434=CARTESIAN_POINT('',(1.775,10.8,5.));
#10435=CARTESIAN_POINT('',(1.775,10.8,5.));
#10436=CARTESIAN_POINT('Origin',(2.,10.8,5.));
#10437=CARTESIAN_POINT('Origin',(2.,10.8,5.));
#10438=CARTESIAN_POINT('',(1.2,11.,5.));
#10439=CARTESIAN_POINT('Origin',(2.,11.,5.));
#10440=CARTESIAN_POINT('',(1.2,10.8,5.));
#10441=CARTESIAN_POINT('',(1.2,10.8,5.));
#10442=CARTESIAN_POINT('Origin',(2.,10.8,5.));
#10443=CARTESIAN_POINT('Origin',(2.,11.,5.));
#10444=CARTESIAN_POINT('Origin',(2.,10.8,5.));
#10445=CARTESIAN_POINT('',(0.,0.,0.));
#10446=CARTESIAN_POINT('Origin',(0.0866025403784439,-0.4,-0.15));
#10447=CARTESIAN_POINT('',(0.173205080756888,-0.4,0.));
#10448=CARTESIAN_POINT('',(0.0866025403784439,-0.4,-0.15));
#10449=CARTESIAN_POINT('',(0.173205080756888,-0.4,0.));
#10450=CARTESIAN_POINT('',(0.0866025403784439,-0.64,-0.15));
#10451=CARTESIAN_POINT('',(0.0866025403784439,-0.4,-0.15));
#10452=CARTESIAN_POINT('',(0.173205080756888,-0.64,0.));
#10453=CARTESIAN_POINT('',(0.173205080756888,-0.64,0.));
#10454=CARTESIAN_POINT('',(0.173205080756888,-0.4,0.));
#10455=CARTESIAN_POINT('Origin',(-0.0866025403784438,-0.4,-0.15));
#10456=CARTESIAN_POINT('',(-0.0866025403784438,-0.4,-0.15));
#10457=CARTESIAN_POINT('',(0.0866025403784439,-0.4,-0.15));
#10458=CARTESIAN_POINT('',(-0.0866025403784438,-0.64,-0.15));
#10459=CARTESIAN_POINT('',(-0.0866025403784438,-0.4,-0.15));
#10460=CARTESIAN_POINT('',(0.0866025403784439,-0.64,-0.15));
#10461=CARTESIAN_POINT('Origin',(-0.173205080756888,-0.4,-2.77555756156289E-17));
#10462=CARTESIAN_POINT('',(-0.173205080756888,-0.4,-2.12115047744981E-17));
#10463=CARTESIAN_POINT('',(-0.0866025403784438,-0.4,-0.15));
#10464=CARTESIAN_POINT('',(-0.173205080756888,-0.64,-2.77555756156289E-17));
#10465=CARTESIAN_POINT('',(-0.173205080756888,-0.4,-2.12115047744981E-17));
#10466=CARTESIAN_POINT('',(-0.0866025403784438,-0.64,-0.15));
#10467=CARTESIAN_POINT('Origin',(-0.0866025403784439,-0.4,0.15));
#10468=CARTESIAN_POINT('',(-0.0866025403784439,-0.4,0.15));
#10469=CARTESIAN_POINT('',(-0.173205080756888,-0.4,-2.12115047744981E-17));
#10470=CARTESIAN_POINT('',(-0.0866025403784439,-0.64,0.15));
#10471=CARTESIAN_POINT('',(-0.0866025403784439,-0.4,0.15));
#10472=CARTESIAN_POINT('',(-0.173205080756888,-0.64,-2.12115047744981E-17));
#10473=CARTESIAN_POINT('Origin',(0.0866025403784439,-0.4,0.15));
#10474=CARTESIAN_POINT('',(0.0866025403784439,-0.4,0.15));
#10475=CARTESIAN_POINT('',(-0.0866025403784439,-0.4,0.15));
#10476=CARTESIAN_POINT('',(0.0866025403784439,-0.64,0.15));
#10477=CARTESIAN_POINT('',(0.0866025403784439,-0.4,0.15));
#10478=CARTESIAN_POINT('',(-0.0866025403784439,-0.64,0.15));
#10479=CARTESIAN_POINT('Origin',(0.173205080756888,-0.4,0.));
#10480=CARTESIAN_POINT('',(0.0866025403784439,-0.4,0.15));
#10481=CARTESIAN_POINT('',(0.0866025403784439,-0.64,0.15));
#10482=CARTESIAN_POINT('Origin',(0.,-0.4,-2.77555756156289E-17));
#10483=CARTESIAN_POINT('Origin',(0.,-0.64,-2.77555756156289E-17));
#10484=CARTESIAN_POINT('Origin',(0.,-1.,0.));
#10485=CARTESIAN_POINT('',(-0.1954,-1.,2.39295984553393E-17));
#10486=CARTESIAN_POINT('Origin',(0.,-1.,0.));
#10487=CARTESIAN_POINT('Origin',(0.3,0.4,0.));
#10488=CARTESIAN_POINT('',(-0.3,0.4,-3.67394039744206E-17));
#10489=CARTESIAN_POINT('Origin',(0.,0.4,0.));
#10490=CARTESIAN_POINT('Origin',(0.,0.375,0.));
#10491=CARTESIAN_POINT('',(-0.35,0.35,-4.28626379701573E-17));
#10492=CARTESIAN_POINT('Origin',(0.,0.35,0.));
#10493=CARTESIAN_POINT('',(-0.325,0.375,-3.9801020972289E-17));
#10494=CARTESIAN_POINT('Origin',(0.,0.19,0.));
#10495=CARTESIAN_POINT('',(-0.35,0.03,-4.28626379701574E-17));
#10496=CARTESIAN_POINT('Origin',(0.,0.03,0.));
#10497=CARTESIAN_POINT('',(-0.35,0.19,-4.28626379701574E-17));
#10498=CARTESIAN_POINT('Origin',(0.,0.0149999999999999,0.));
#10499=CARTESIAN_POINT('',(-0.32,-3.29597460435593E-17,-3.91886975727153E-17));
#10500=CARTESIAN_POINT('Origin',(0.,0.,0.));
#10501=CARTESIAN_POINT('',(-0.335,0.0149999999999999,-4.10256677714363E-17));
#10502=CARTESIAN_POINT('Origin',(0.22,0.,0.));
#10503=CARTESIAN_POINT('',(-0.22,-6.93889390390723E-18,-2.69422295812418E-17));
#10504=CARTESIAN_POINT('Origin',(0.,0.,0.));
#10505=CARTESIAN_POINT('Origin',(0.,-0.02,0.));
#10506=CARTESIAN_POINT('',(-0.1954,-0.0492,2.39295984553393E-17));
#10507=CARTESIAN_POINT('Origin',(0.,-0.0492,0.));
#10508=CARTESIAN_POINT('',(-0.21,-0.02,-2.57175827820944E-17));
#10509=CARTESIAN_POINT('Origin',(0.,-0.8,0.));
#10510=CARTESIAN_POINT('',(-0.1954,-0.8,-2.39295984553393E-17));
#10511=CARTESIAN_POINT('',(0.,0.,0.));
#10512=CARTESIAN_POINT('Origin',(5.,0.,3.8));
#10513=CARTESIAN_POINT('',(4.4,-7.34788079488412E-17,13.8));
#10514=CARTESIAN_POINT('Origin',(5.,0.,13.8));
#10515=CARTESIAN_POINT('',(4.4,-7.34788079488412E-17,3.8));
#10516=CARTESIAN_POINT('',(4.4,-7.34788079488412E-17,3.8));
#10517=CARTESIAN_POINT('Origin',(5.,0.,3.8));
#10518=CARTESIAN_POINT('Origin',(5.,0.,13.8));
#10519=CARTESIAN_POINT('Origin',(5.,-1.2,2.7));
#10520=CARTESIAN_POINT('',(4.725,-1.2,2.8));
#10521=CARTESIAN_POINT('Origin',(5.,-1.2,2.8));
#10522=CARTESIAN_POINT('',(4.725,-1.2,3.8));
#10523=CARTESIAN_POINT('',(4.725,-1.2,2.7));
#10524=CARTESIAN_POINT('Origin',(5.,-1.2,3.8));
#10525=CARTESIAN_POINT('Origin',(5.,1.2,2.7));
#10526=CARTESIAN_POINT('',(4.725,1.2,2.8));
#10527=CARTESIAN_POINT('Origin',(5.,1.2,2.8));
#10528=CARTESIAN_POINT('',(4.725,1.2,3.8));
#10529=CARTESIAN_POINT('',(4.725,1.2,2.7));
#10530=CARTESIAN_POINT('Origin',(5.,1.2,3.8));
#10531=CARTESIAN_POINT('Origin',(6.,2.,2.8));
#10532=CARTESIAN_POINT('',(6.,2.,2.8));
#10533=CARTESIAN_POINT('',(4.,2.,2.8));
#10534=CARTESIAN_POINT('',(6.,2.,2.8));
#10535=CARTESIAN_POINT('',(4.,2.,3.8));
#10536=CARTESIAN_POINT('',(4.,2.,2.8));
#10537=CARTESIAN_POINT('',(6.,2.,3.8));
#10538=CARTESIAN_POINT('',(6.,2.,3.8));
#10539=CARTESIAN_POINT('',(6.,2.,2.8));
#10540=CARTESIAN_POINT('Origin',(6.,-2.,2.8));
#10541=CARTESIAN_POINT('',(6.,-2.,2.8));
#10542=CARTESIAN_POINT('',(6.,-2.,2.8));
#10543=CARTESIAN_POINT('',(6.,-2.,3.8));
#10544=CARTESIAN_POINT('',(6.,-2.,3.8));
#10545=CARTESIAN_POINT('',(6.,-2.,2.8));
#10546=CARTESIAN_POINT('Origin',(4.,-2.,2.8));
#10547=CARTESIAN_POINT('',(4.,-2.,2.8));
#10548=CARTESIAN_POINT('',(4.,-2.,2.8));
#10549=CARTESIAN_POINT('',(4.,-2.,3.8));
#10550=CARTESIAN_POINT('',(4.,-2.,3.8));
#10551=CARTESIAN_POINT('',(4.,-2.,2.8));
#10552=CARTESIAN_POINT('Origin',(4.,2.,2.8));
#10553=CARTESIAN_POINT('',(4.,2.,2.8));
#10554=CARTESIAN_POINT('',(4.,2.,3.8));
#10555=CARTESIAN_POINT('Origin',(5.,0.,3.8));
#10556=CARTESIAN_POINT('Origin',(5.,0.,2.8));
#10557=CARTESIAN_POINT('',(0.,0.,0.));
#10558=CARTESIAN_POINT('Origin',(0.115470053837925,-0.5,-0.2));
#10559=CARTESIAN_POINT('',(0.23094010767585,-0.5,0.));
#10560=CARTESIAN_POINT('',(0.115470053837925,-0.5,-0.2));
#10561=CARTESIAN_POINT('',(0.23094010767585,-0.5,0.));
#10562=CARTESIAN_POINT('',(0.115470053837925,-0.8,-0.2));
#10563=CARTESIAN_POINT('',(0.115470053837925,-0.5,-0.2));
#10564=CARTESIAN_POINT('',(0.23094010767585,-0.8,0.));
#10565=CARTESIAN_POINT('',(0.23094010767585,-0.8,0.));
#10566=CARTESIAN_POINT('',(0.23094010767585,-0.5,0.));
#10567=CARTESIAN_POINT('Origin',(-0.115470053837925,-0.5,-0.2));
#10568=CARTESIAN_POINT('',(-0.115470053837925,-0.5,-0.2));
#10569=CARTESIAN_POINT('',(0.115470053837925,-0.5,-0.2));
#10570=CARTESIAN_POINT('',(-0.115470053837925,-0.8,-0.2));
#10571=CARTESIAN_POINT('',(-0.115470053837925,-0.5,-0.2));
#10572=CARTESIAN_POINT('',(0.115470053837925,-0.8,-0.2));
#10573=CARTESIAN_POINT('Origin',(-0.23094010767585,-0.5,-2.77555756156289E-17));
#10574=CARTESIAN_POINT('',(-0.23094010767585,-0.5,-2.82820063659975E-17));
#10575=CARTESIAN_POINT('',(-0.115470053837925,-0.5,-0.2));
#10576=CARTESIAN_POINT('',(-0.23094010767585,-0.8,-2.77555756156289E-17));
#10577=CARTESIAN_POINT('',(-0.23094010767585,-0.5,-2.82820063659975E-17));
#10578=CARTESIAN_POINT('',(-0.115470053837925,-0.8,-0.2));
#10579=CARTESIAN_POINT('Origin',(-0.115470053837925,-0.5,0.2));
#10580=CARTESIAN_POINT('',(-0.115470053837925,-0.5,0.2));
#10581=CARTESIAN_POINT('',(-0.23094010767585,-0.5,-2.82820063659975E-17));
#10582=CARTESIAN_POINT('',(-0.115470053837925,-0.8,0.2));
#10583=CARTESIAN_POINT('',(-0.115470053837925,-0.5,0.2));
#10584=CARTESIAN_POINT('',(-0.23094010767585,-0.8,-2.82820063659975E-17));
#10585=CARTESIAN_POINT('Origin',(0.115470053837925,-0.5,0.2));
#10586=CARTESIAN_POINT('',(0.115470053837925,-0.5,0.2));
#10587=CARTESIAN_POINT('',(-0.115470053837925,-0.5,0.2));
#10588=CARTESIAN_POINT('',(0.115470053837925,-0.8,0.2));
#10589=CARTESIAN_POINT('',(0.115470053837925,-0.5,0.2));
#10590=CARTESIAN_POINT('',(-0.115470053837925,-0.8,0.2));
#10591=CARTESIAN_POINT('Origin',(0.23094010767585,-0.5,0.));
#10592=CARTESIAN_POINT('',(0.115470053837925,-0.5,0.2));
#10593=CARTESIAN_POINT('',(0.115470053837925,-0.8,0.2));
#10594=CARTESIAN_POINT('Origin',(0.,-0.5,0.));
#10595=CARTESIAN_POINT('Origin',(0.,-0.8,0.));
#10596=CARTESIAN_POINT('Origin',(0.,-1.4,0.));
#10597=CARTESIAN_POINT('',(-0.24505,-1.4,3.00099698131059E-17));
#10598=CARTESIAN_POINT('Origin',(0.,-1.4,0.));
#10599=CARTESIAN_POINT('Origin',(0.375,0.5,0.));
#10600=CARTESIAN_POINT('',(-0.375,0.5,-4.59242549680257E-17));
#10601=CARTESIAN_POINT('Origin',(0.,0.5,0.));
#10602=CARTESIAN_POINT('Origin',(0.,0.475,0.));
#10603=CARTESIAN_POINT('',(-0.425,0.45,-5.20474889637625E-17));
#10604=CARTESIAN_POINT('Origin',(0.,0.45,0.));
#10605=CARTESIAN_POINT('',(-0.4,0.475,-4.89858719658941E-17));
#10606=CARTESIAN_POINT('Origin',(0.,0.24,0.));
#10607=CARTESIAN_POINT('',(-0.425,0.0299999999999998,-5.20474889637625E-17));
#10608=CARTESIAN_POINT('Origin',(0.,0.0299999999999998,0.));
#10609=CARTESIAN_POINT('',(-0.425,0.24,-5.20474889637625E-17));
#10610=CARTESIAN_POINT('Origin',(0.,0.0150000000000001,0.));
#10611=CARTESIAN_POINT('',(-0.395,4.85722573273506E-17,-4.83735485663204E-17));
#10612=CARTESIAN_POINT('Origin',(0.,0.,0.));
#10613=CARTESIAN_POINT('',(-0.41,0.0150000000000001,-5.02105187650415E-17));
#10614=CARTESIAN_POINT('Origin',(0.27,0.,0.));
#10615=CARTESIAN_POINT('',(-0.27,0.,-3.30654635769785E-17));
#10616=CARTESIAN_POINT('Origin',(0.,0.,0.));
#10617=CARTESIAN_POINT('Origin',(0.,-0.02,0.));
#10618=CARTESIAN_POINT('',(-0.24505,-0.0498999999999999,3.00099698131059E-17));
#10619=CARTESIAN_POINT('Origin',(0.,-0.0498999999999999,0.));
#10620=CARTESIAN_POINT('',(-0.26,-0.02,-3.18408167778312E-17));
#10621=CARTESIAN_POINT('Origin',(0.,-0.995,0.));
#10622=CARTESIAN_POINT('',(-0.24505,-0.995,-3.00099698131059E-17));
#10623=CARTESIAN_POINT('',(0.,0.,0.));
#10624=CARTESIAN_POINT('Origin',(0.,0.39,12.6));
#10625=CARTESIAN_POINT('',(-0.088881944173156,0.39,12.4097370240956));
#10626=CARTESIAN_POINT('',(-0.088881944173156,0.39,12.7902629759044));
#10627=CARTESIAN_POINT('',(-0.088881944173156,0.39,11.9));
#10628=CARTESIAN_POINT('',(-0.21,0.39,12.6));
#10629=CARTESIAN_POINT('Origin',(0.,0.39,12.6));
#10630=CARTESIAN_POINT('Origin',(0.,0.39,12.6));
#10631=CARTESIAN_POINT('Origin',(0.,0.39,12.6));
#10632=CARTESIAN_POINT('',(0.088881944173156,0.39,12.4097370240956));
#10633=CARTESIAN_POINT('Ctrl Pts',(0.088881944173156,0.39,12.4097370240956));
#10634=CARTESIAN_POINT('Ctrl Pts',(0.086315498079388,0.390584899278025,
12.4085381007772));
#10635=CARTESIAN_POINT('Ctrl Pts',(0.0837209983713384,0.391149522707465,
12.4073893629036));
#10636=CARTESIAN_POINT('Ctrl Pts',(0.0552990416535447,0.397034429112172,
12.3954896015193));
#10637=CARTESIAN_POINT('Ctrl Pts',(0.0269260609044579,0.4,12.39));
#10638=CARTESIAN_POINT('Ctrl Pts',(-0.0269260609044578,0.4,12.39));
#10639=CARTESIAN_POINT('Ctrl Pts',(-0.0552990416535446,0.397034429112172,
12.3954896015193));
#10640=CARTESIAN_POINT('Ctrl Pts',(-0.0837209983713383,0.391149522707465,
12.4073893629036));
#10641=CARTESIAN_POINT('Ctrl Pts',(-0.086315498079388,0.390584899278025,
12.4085381007772));
#10642=CARTESIAN_POINT('Ctrl Pts',(-0.088881944173156,0.39,12.4097370240956));
#10643=CARTESIAN_POINT('',(0.088881944173156,0.39,12.7902629759044));
#10644=CARTESIAN_POINT('Origin',(0.,0.39,12.6));
#10645=CARTESIAN_POINT('Ctrl Pts',(-0.088881944173156,0.39,12.7902629759044));
#10646=CARTESIAN_POINT('Ctrl Pts',(-0.0863154980793892,0.390584899278025,
12.7914618992227));
#10647=CARTESIAN_POINT('Ctrl Pts',(-0.0837209983713384,0.391149522707465,
12.7926106370964));
#10648=CARTESIAN_POINT('Ctrl Pts',(-0.0552990416535446,0.397034429112172,
12.8045103984807));
#10649=CARTESIAN_POINT('Ctrl Pts',(-0.0269260609044578,0.4,12.81));
#10650=CARTESIAN_POINT('Ctrl Pts',(0.0269260609044579,0.4,12.81));
#10651=CARTESIAN_POINT('Ctrl Pts',(0.0552990416535447,0.397034429112172,
12.8045103984807));
#10652=CARTESIAN_POINT('Ctrl Pts',(0.0837209983713384,0.391149522707465,
12.7926106370964));
#10653=CARTESIAN_POINT('Ctrl Pts',(0.0863154980793892,0.390584899278025,
12.7914618992227));
#10654=CARTESIAN_POINT('Ctrl Pts',(0.088881944173156,0.39,12.7902629759044));
#10655=CARTESIAN_POINT('',(-0.21,1.,12.6));
#10656=CARTESIAN_POINT('',(-0.21,0.39,12.6));
#10657=CARTESIAN_POINT('Origin',(0.,1.,12.6));
#10658=CARTESIAN_POINT('Origin',(0.,0.39,12.6));
#10659=CARTESIAN_POINT('',(0.088881944173156,0.39,11.9));
#10660=CARTESIAN_POINT('Origin',(5.,0.58,12.6));
#10661=CARTESIAN_POINT('',(4.82788085521941,0.58,12.4796879058448));
#10662=CARTESIAN_POINT('',(4.82788085521941,0.58,12.7203120941552));
#10663=CARTESIAN_POINT('',(4.82788085521941,0.58,11.9));
#10664=CARTESIAN_POINT('',(4.79,0.58,12.6));
#10665=CARTESIAN_POINT('Origin',(5.,0.58,12.6));
#10666=CARTESIAN_POINT('Origin',(5.,0.58,12.6));
#10667=CARTESIAN_POINT('Origin',(5.,0.58,12.6));
#10668=CARTESIAN_POINT('',(5.17211914478059,0.58,12.4796879058448));
#10669=CARTESIAN_POINT('Ctrl Pts',(5.17211914478059,0.58,12.4796879058448));
#10670=CARTESIAN_POINT('Ctrl Pts',(5.16494300386906,0.582129571097444,12.4694216791185));
#10671=CARTESIAN_POINT('Ctrl Pts',(5.15694888384172,0.584352756238741,12.4599640357434));
#10672=CARTESIAN_POINT('Ctrl Pts',(5.12997632363586,0.591181849259721,12.4329914755375));
#10673=CARTESIAN_POINT('Ctrl Pts',(5.10650870388547,0.596121344050056,12.4168630281897));
#10674=CARTESIAN_POINT('Ctrl Pts',(5.05482987213252,0.603074162899704,12.3953614389456));
#10675=CARTESIAN_POINT('Ctrl Pts',(5.02660205959229,0.605,12.39));
#10676=CARTESIAN_POINT('Ctrl Pts',(4.97339794040771,0.605,12.39));
#10677=CARTESIAN_POINT('Ctrl Pts',(4.94517012786748,0.603074162899704,12.3953614389456));
#10678=CARTESIAN_POINT('Ctrl Pts',(4.89349129611453,0.596121344050056,12.4168630281897));
#10679=CARTESIAN_POINT('Ctrl Pts',(4.87002367636414,0.591181849259721,12.4329914755375));
#10680=CARTESIAN_POINT('Ctrl Pts',(4.84305111615828,0.584352756238741,12.4599640357434));
#10681=CARTESIAN_POINT('Ctrl Pts',(4.83505699613094,0.582129571097444,12.4694216791185));
#10682=CARTESIAN_POINT('Ctrl Pts',(4.82788085521941,0.58,12.4796879058448));
#10683=CARTESIAN_POINT('',(5.17211914478059,0.58,12.7203120941552));
#10684=CARTESIAN_POINT('Origin',(5.,0.58,12.6));
#10685=CARTESIAN_POINT('Ctrl Pts',(4.82788085521941,0.58,12.7203120941552));
#10686=CARTESIAN_POINT('Ctrl Pts',(4.83505699613094,0.582129571097444,12.7305783208815));
#10687=CARTESIAN_POINT('Ctrl Pts',(4.84305111615828,0.584352756238741,12.7400359642566));
#10688=CARTESIAN_POINT('Ctrl Pts',(4.87002367636414,0.591181849259721,12.7670085244625));
#10689=CARTESIAN_POINT('Ctrl Pts',(4.89349129611453,0.596121344050056,12.7831369718103));
#10690=CARTESIAN_POINT('Ctrl Pts',(4.94517012786748,0.603074162899704,12.8046385610544));
#10691=CARTESIAN_POINT('Ctrl Pts',(4.97339794040771,0.605,12.81));
#10692=CARTESIAN_POINT('Ctrl Pts',(5.02660205959229,0.605,12.81));
#10693=CARTESIAN_POINT('Ctrl Pts',(5.05482987213252,0.603074162899704,12.8046385610544));
#10694=CARTESIAN_POINT('Ctrl Pts',(5.10650870388547,0.596121344050056,12.7831369718103));
#10695=CARTESIAN_POINT('Ctrl Pts',(5.12997632363586,0.591181849259721,12.7670085244625));
#10696=CARTESIAN_POINT('Ctrl Pts',(5.15694888384172,0.584352756238741,12.7400359642566));
#10697=CARTESIAN_POINT('Ctrl Pts',(5.16494300386906,0.582129571097444,12.7305783208815));
#10698=CARTESIAN_POINT('Ctrl Pts',(5.17211914478059,0.58,12.7203120941552));
#10699=CARTESIAN_POINT('',(4.79,1.,12.6));
#10700=CARTESIAN_POINT('',(4.79,0.58,12.6));
#10701=CARTESIAN_POINT('Origin',(5.,1.,12.6));
#10702=CARTESIAN_POINT('Origin',(5.,0.58,12.6));
#10703=CARTESIAN_POINT('',(5.17211914478059,0.58,11.9));
#10704=CARTESIAN_POINT('Origin',(0.,0.,11.9));
#10705=CARTESIAN_POINT('',(-0.4,-4.89858719658941E-17,12.));
#10706=CARTESIAN_POINT('Origin',(0.,0.,12.));
#10707=CARTESIAN_POINT('',(-0.4,4.89858719658941E-17,13.2));
#10708=CARTESIAN_POINT('',(-0.4,-4.89858719658941E-17,11.9));
#10709=CARTESIAN_POINT('Origin',(0.,0.,13.2));
#10710=CARTESIAN_POINT('Origin',(5.,0.,11.9));
#10711=CARTESIAN_POINT('',(4.395,-7.40911313484149E-17,12.));
#10712=CARTESIAN_POINT('Origin',(5.,0.,12.));
#10713=CARTESIAN_POINT('',(4.395,7.40911313484149E-17,13.2));
#10714=CARTESIAN_POINT('',(4.395,-7.40911313484149E-17,11.9));
#10715=CARTESIAN_POINT('Origin',(5.,0.,13.2));
#10716=CARTESIAN_POINT('Origin',(6.,1.,12.));
#10717=CARTESIAN_POINT('',(6.,1.,12.));
#10718=CARTESIAN_POINT('',(-1.,1.,12.));
#10719=CARTESIAN_POINT('',(6.,1.,12.));
#10720=CARTESIAN_POINT('',(-1.,1.,13.2));
#10721=CARTESIAN_POINT('',(-1.,1.,12.));
#10722=CARTESIAN_POINT('',(6.,1.,13.2));
#10723=CARTESIAN_POINT('',(6.,1.,13.2));
#10724=CARTESIAN_POINT('',(6.,1.,12.));
#10725=CARTESIAN_POINT('Origin',(6.,-1.,12.));
#10726=CARTESIAN_POINT('',(6.,-1.,12.));
#10727=CARTESIAN_POINT('',(6.,-1.,12.));
#10728=CARTESIAN_POINT('',(6.,-1.,13.2));
#10729=CARTESIAN_POINT('',(6.,-1.,13.2));
#10730=CARTESIAN_POINT('',(6.,-1.,12.));
#10731=CARTESIAN_POINT('Origin',(-1.,-1.,12.));
#10732=CARTESIAN_POINT('',(-1.,-1.,12.));
#10733=CARTESIAN_POINT('',(-1.,-1.,12.));
#10734=CARTESIAN_POINT('',(-1.,-1.,13.2));
#10735=CARTESIAN_POINT('',(-1.,-1.,13.2));
#10736=CARTESIAN_POINT('',(-1.,-1.,12.));
#10737=CARTESIAN_POINT('Origin',(-1.,1.,12.));
#10738=CARTESIAN_POINT('',(-1.,1.,12.));
#10739=CARTESIAN_POINT('',(-1.,1.,13.2));
#10740=CARTESIAN_POINT('Origin',(2.5,0.,13.2));
#10741=CARTESIAN_POINT('Origin',(2.5,0.,12.));
#10742=CARTESIAN_POINT('',(0.,0.,0.));
#10743=CARTESIAN_POINT('Origin',(0.0721687836487032,0.,-0.125));
#10744=CARTESIAN_POINT('',(0.0721687836487032,0.,-0.125));
#10745=CARTESIAN_POINT('',(0.144337567297406,0.,0.));
#10746=CARTESIAN_POINT('',(0.117710979560879,0.,-0.0461186027918559));
#10747=CARTESIAN_POINT('',(0.0721687836487032,-0.25,-0.125));
#10748=CARTESIAN_POINT('',(0.0721687836487032,0.,-0.125));
#10749=CARTESIAN_POINT('',(0.144337567297406,-0.25,0.));
#10750=CARTESIAN_POINT('',(0.144337567297406,-0.25,0.));
#10751=CARTESIAN_POINT('',(0.144337567297406,0.,0.));
#10752=CARTESIAN_POINT('Origin',(-0.0721687836487032,0.,-0.125));
#10753=CARTESIAN_POINT('',(-0.0721687836487032,0.,-0.125));
#10754=CARTESIAN_POINT('',(0.0739156081756484,0.,-0.125));
#10755=CARTESIAN_POINT('',(-0.0721687836487032,-0.25,-0.125));
#10756=CARTESIAN_POINT('',(-0.0721687836487032,0.,-0.125));
#10757=CARTESIAN_POINT('',(0.0721687836487032,-0.25,-0.125));
#10758=CARTESIAN_POINT('Origin',(-0.144337567297406,0.,-4.16333634234434E-17));
#10759=CARTESIAN_POINT('',(-0.144337567297406,0.,-1.76762539787485E-17));
#10760=CARTESIAN_POINT('',(-0.0987953713852306,0.,-0.0788813972081442));
#10761=CARTESIAN_POINT('',(-0.144337567297406,-0.25,-2.77555756156289E-17));
#10762=CARTESIAN_POINT('',(-0.144337567297406,0.,-1.76762539787485E-17));
#10763=CARTESIAN_POINT('',(-0.0721687836487032,-0.25,-0.125));
#10764=CARTESIAN_POINT('Origin',(-0.0721687836487033,0.,0.125));
#10765=CARTESIAN_POINT('',(-0.0721687836487033,0.,0.125));
#10766=CARTESIAN_POINT('',(-0.0627109795608791,0.,0.141381397208144));
#10767=CARTESIAN_POINT('',(-0.0721687836487033,-0.25,0.125));
#10768=CARTESIAN_POINT('',(-0.0721687836487033,0.,0.125));
#10769=CARTESIAN_POINT('',(-0.144337567297406,-0.25,-1.76762539787485E-17));
#10770=CARTESIAN_POINT('Origin',(0.0721687836487032,0.,0.125));
#10771=CARTESIAN_POINT('',(0.0721687836487032,0.,0.125));
#10772=CARTESIAN_POINT('',(0.146084391824352,0.,0.125));
#10773=CARTESIAN_POINT('',(0.0721687836487032,-0.25,0.125));
#10774=CARTESIAN_POINT('',(0.0721687836487032,0.,0.125));
#10775=CARTESIAN_POINT('',(-0.0721687836487033,-0.25,0.125));
#10776=CARTESIAN_POINT('Origin',(0.144337567297406,0.,0.));
#10777=CARTESIAN_POINT('',(0.153795371385231,0.,-0.0163813972081441));
#10778=CARTESIAN_POINT('',(0.0721687836487032,-0.25,0.125));
#10779=CARTESIAN_POINT('Origin',(0.,-0.25,0.));
#10780=CARTESIAN_POINT('Origin',(0.22,0.,0.));
#10781=CARTESIAN_POINT('',(-0.22,-8.67361737988404E-18,-2.69422295812418E-17));
#10782=CARTESIAN_POINT('Origin',(0.,0.,0.));
#10783=CARTESIAN_POINT('Origin',(0.,-0.015,0.));
#10784=CARTESIAN_POINT('',(-0.24505,-0.02505,-3.00099698131059E-17));
#10785=CARTESIAN_POINT('Origin',(0.,-0.02505,0.));
#10786=CARTESIAN_POINT('',(-0.235,-0.015,-2.87791997799628E-17));
#10787=CARTESIAN_POINT('Origin',(0.,-0.3775,0.));
#10788=CARTESIAN_POINT('',(-0.24505,-0.72995,3.00099698131059E-17));
#10789=CARTESIAN_POINT('Origin',(0.,-0.72995,0.));
#10790=CARTESIAN_POINT('',(-0.24505,-0.3775,-3.00099698131059E-17));
#10791=CARTESIAN_POINT('Origin',(0.,-0.7625,0.));
#10792=CARTESIAN_POINT('',(-0.175,-0.8,-2.14313189850787E-17));
#10793=CARTESIAN_POINT('Origin',(0.,-0.8,0.));
#10794=CARTESIAN_POINT('',(-0.2125,-0.7625,-2.60237444818813E-17));
#10795=CARTESIAN_POINT('Origin',(0.,-0.8,0.));
#10796=CARTESIAN_POINT('',(0.,0.,0.));
#10797=CARTESIAN_POINT('Origin',(0.,0.,9.9));
#10798=CARTESIAN_POINT('',(-0.15,-1.83697019872103E-17,10.));
#10799=CARTESIAN_POINT('Origin',(0.,0.,10.));
#10800=CARTESIAN_POINT('',(-0.15,-1.83697019872103E-17,13.9));
#10801=CARTESIAN_POINT('',(-0.15,-1.83697019872103E-17,9.9));
#10802=CARTESIAN_POINT('Origin',(0.,0.,13.9));
#10803=CARTESIAN_POINT('Origin',(0.,0.,13.9));
#10804=CARTESIAN_POINT('Origin',(0.,0.,10.));
#10805=CARTESIAN_POINT('',(0.4,-4.16333634234434E-17,13.4450071225216));
#10806=CARTESIAN_POINT('',(-0.4,-4.89858719658941E-17,13.4450071225216));
#10807=CARTESIAN_POINT('Ctrl Pts',(0.4,-4.16333634234434E-17,13.4450071225216));
#10808=CARTESIAN_POINT('Ctrl Pts',(0.4,0.0504086500787391,13.4450071225216));
#10809=CARTESIAN_POINT('Ctrl Pts',(0.389891257329757,0.10405747970835,13.4426096554494));
#10810=CARTESIAN_POINT('Ctrl Pts',(0.349018656101199,0.202556511873035,
13.4340379438059));
#10811=CARTESIAN_POINT('Ctrl Pts',(0.318263533348268,0.24742189160097,13.4279969749484));
#10812=CARTESIAN_POINT('Ctrl Pts',(0.247424944224197,0.318260480725041,
13.4167257438327));
#10813=CARTESIAN_POINT('Ctrl Pts',(0.202558278587653,0.349017990321186,
13.4107505468858));
#10814=CARTESIAN_POINT('Ctrl Pts',(0.104054739507664,0.389892327061432,
13.4023303772031));
#10815=CARTESIAN_POINT('Ctrl Pts',(0.0504043057803212,0.4,13.4));
#10816=CARTESIAN_POINT('Ctrl Pts',(-0.0504043057803211,0.4,13.4));
#10817=CARTESIAN_POINT('Ctrl Pts',(-0.104054739507664,0.389892327061432,
13.4023303772031));
#10818=CARTESIAN_POINT('Ctrl Pts',(-0.202558278587653,0.349017990321186,
13.4107505468858));
#10819=CARTESIAN_POINT('Ctrl Pts',(-0.247424944224197,0.318260480725041,
13.4167257438327));
#10820=CARTESIAN_POINT('Ctrl Pts',(-0.318263533348268,0.24742189160097,
13.4279969749484));
#10821=CARTESIAN_POINT('Ctrl Pts',(-0.349018656101199,0.202556511873035,
13.4340379438059));
#10822=CARTESIAN_POINT('Ctrl Pts',(-0.389891257329757,0.10405747970835,
13.4426096554494));
#10823=CARTESIAN_POINT('Ctrl Pts',(-0.4,0.0504086500787392,13.4450071225216));
#10824=CARTESIAN_POINT('Ctrl Pts',(-0.4,1.38777878078145E-17,13.4450071225216));
#10825=CARTESIAN_POINT('Ctrl Pts',(-0.4,5.55111512312578E-17,13.4450071225216));
#10826=CARTESIAN_POINT('Ctrl Pts',(-0.4,-0.0504086500787391,13.4450071225216));
#10827=CARTESIAN_POINT('Ctrl Pts',(-0.389891257329757,-0.10405747970835,
13.4426096554494));
#10828=CARTESIAN_POINT('Ctrl Pts',(-0.349018656101199,-0.202556511873035,
13.4340379438059));
#10829=CARTESIAN_POINT('Ctrl Pts',(-0.318263533348268,-0.24742189160097,
13.4279969749484));
#10830=CARTESIAN_POINT('Ctrl Pts',(-0.247424944224197,-0.318260480725041,
13.4167257438327));
#10831=CARTESIAN_POINT('Ctrl Pts',(-0.202558278587653,-0.349017990321186,
13.4107505468858));
#10832=CARTESIAN_POINT('Ctrl Pts',(-0.104054739507664,-0.389892327061432,
13.4023303772031));
#10833=CARTESIAN_POINT('Ctrl Pts',(-0.0504043057803212,-0.4,13.4));
#10834=CARTESIAN_POINT('Ctrl Pts',(0.050404305780321,-0.4,13.4));
#10835=CARTESIAN_POINT('Ctrl Pts',(0.104054739507664,-0.389892327061432,
13.4023303772031));
#10836=CARTESIAN_POINT('Ctrl Pts',(0.202558278587653,-0.349017990321186,
13.4107505468858));
#10837=CARTESIAN_POINT('Ctrl Pts',(0.247424944224197,-0.318260480725041,
13.4167257438327));
#10838=CARTESIAN_POINT('Ctrl Pts',(0.318263533348268,-0.24742189160097,
13.4279969749484));
#10839=CARTESIAN_POINT('Ctrl Pts',(0.349018656101199,-0.202556511873035,
13.4340379438059));
#10840=CARTESIAN_POINT('Ctrl Pts',(0.389891257329757,-0.10405747970835,
13.4426096554494));
#10841=CARTESIAN_POINT('Ctrl Pts',(0.4,-0.0504086500787392,13.4450071225216));
#10842=CARTESIAN_POINT('Ctrl Pts',(0.4,-1.38777878078145E-17,13.4450071225216));
#10843=CARTESIAN_POINT('',(-0.4,-4.89858719658941E-17,10.));
#10844=CARTESIAN_POINT('',(-0.4,-4.89858719658941E-17,10.));
#10845=CARTESIAN_POINT('Origin',(0.,0.,10.));
#10846=CARTESIAN_POINT('Origin',(0.,0.,10.));
#10847=CARTESIAN_POINT('Origin',(0.,-0.6,15.2));
#10848=CARTESIAN_POINT('',(-1.8,0.6,15.2));
#10849=CARTESIAN_POINT('Origin',(0.,0.6,15.2));
#10850=CARTESIAN_POINT('',(-1.8,-0.6,15.2));
#10851=CARTESIAN_POINT('',(-1.8,-0.6,15.2));
#10852=CARTESIAN_POINT('Origin',(0.,-0.6,15.2));
#10853=CARTESIAN_POINT('Origin',(0.,0.6,15.2));
#10854=CARTESIAN_POINT('Origin',(0.,-0.6,15.2));
#10855=CARTESIAN_POINT('',(0.,0.,0.));
#10856=CARTESIAN_POINT('Origin',(0.,0.6,15.2));
#10857=CARTESIAN_POINT('',(-1.6,0.7,15.2));
#10858=CARTESIAN_POINT('Origin',(0.,0.7,15.2));
#10859=CARTESIAN_POINT('',(-1.6,0.6,15.2));
#10860=CARTESIAN_POINT('',(-1.6,0.6,15.2));
#10861=CARTESIAN_POINT('Origin',(0.,0.6,15.2));
#10862=CARTESIAN_POINT('Origin',(0.,0.7,15.2));
#10863=CARTESIAN_POINT('Origin',(0.,0.6,15.2));
#10864=CARTESIAN_POINT('',(0.,0.,0.));
#10865=CARTESIAN_POINT('Origin',(-0.05,0.7,15.2));
#10866=CARTESIAN_POINT('',(0.,0.7,16.5));
#10867=CARTESIAN_POINT('',(-0.05,0.7,15.2));
#10868=CARTESIAN_POINT('',(0.,0.7,16.5));
#10869=CARTESIAN_POINT('',(0.,0.75,16.5));
#10870=CARTESIAN_POINT('',(0.,0.7,16.5));
#10871=CARTESIAN_POINT('',(-0.05,0.75,15.2));
#10872=CARTESIAN_POINT('',(0.,0.75,16.5));
#10873=CARTESIAN_POINT('',(-0.05,0.7,15.2));
#10874=CARTESIAN_POINT('Origin',(0.05,0.7,15.2));
#10875=CARTESIAN_POINT('',(0.05,0.7,15.2));
#10876=CARTESIAN_POINT('',(-0.05,0.7,15.2));
#10877=CARTESIAN_POINT('',(0.05,0.75,15.2));
#10878=CARTESIAN_POINT('',(-0.05,0.75,15.2));
#10879=CARTESIAN_POINT('',(0.05,0.7,15.2));
#10880=CARTESIAN_POINT('Origin',(6.93889390390723E-18,0.7,16.5));
#10881=CARTESIAN_POINT('',(0.05,0.7,15.2));
#10882=CARTESIAN_POINT('',(0.05,0.75,15.2));
#10883=CARTESIAN_POINT('Origin',(-6.93889390390723E-18,0.75,15.85));
#10884=CARTESIAN_POINT('Origin',(-6.93889390390723E-18,0.7,15.85));
#10885=CARTESIAN_POINT('',(0.,0.,0.));
#10886=CARTESIAN_POINT('Origin',(0.,0.,7.95959179));
#10887=CARTESIAN_POINT('',(-0.15,-1.83697019872103E-17,10.));
#10888=CARTESIAN_POINT('Origin',(0.,0.,10.));
#10889=CARTESIAN_POINT('',(-0.15,-1.83697019872103E-17,7.95959179));
#10890=CARTESIAN_POINT('',(-0.15,-1.83697019872103E-17,7.95959179));
#10891=CARTESIAN_POINT('Origin',(0.,0.,7.95959179));
#10892=CARTESIAN_POINT('Origin',(0.,0.,10.));
#10893=CARTESIAN_POINT('Origin',(0.,0.,7.95959179));
#10894=CARTESIAN_POINT('',(0.,0.,0.));
#10895=CARTESIAN_POINT('Origin',(2.,-10.8,5.));
#10896=CARTESIAN_POINT('',(1.495,-10.45,5.));
#10897=CARTESIAN_POINT('Origin',(2.,-10.45,5.));
#10898=CARTESIAN_POINT('',(1.495,-10.8,5.));
#10899=CARTESIAN_POINT('',(1.495,-10.8,5.));
#10900=CARTESIAN_POINT('Origin',(2.,-10.8,5.));
#10901=CARTESIAN_POINT('Origin',(2.,-10.8,5.));
#10902=CARTESIAN_POINT('',(1.3,-10.45,5.));
#10903=CARTESIAN_POINT('Origin',(2.,-10.45,5.));
#10904=CARTESIAN_POINT('',(1.3,-10.8,5.));
#10905=CARTESIAN_POINT('',(1.3,-10.8,5.));
#10906=CARTESIAN_POINT('Origin',(2.,-10.8,5.));
#10907=CARTESIAN_POINT('Origin',(2.,-10.45,5.));
#10908=CARTESIAN_POINT('Origin',(2.,-10.8,5.));
#10909=CARTESIAN_POINT('',(0.,0.,0.));
#10910=CARTESIAN_POINT('Origin',(2.,9.2,5.));
#10911=CARTESIAN_POINT('',(1.495,9.55,5.));
#10912=CARTESIAN_POINT('Origin',(2.,9.55,5.));
#10913=CARTESIAN_POINT('',(1.495,9.2,5.));
#10914=CARTESIAN_POINT('',(1.495,9.2,5.));
#10915=CARTESIAN_POINT('Origin',(2.,9.2,5.));
#10916=CARTESIAN_POINT('Origin',(2.,9.2,5.));
#10917=CARTESIAN_POINT('',(1.3,9.55,5.));
#10918=CARTESIAN_POINT('Origin',(2.,9.55,5.));
#10919=CARTESIAN_POINT('',(1.3,9.2,5.));
#10920=CARTESIAN_POINT('',(1.3,9.2,5.));
#10921=CARTESIAN_POINT('Origin',(2.,9.2,5.));
#10922=CARTESIAN_POINT('Origin',(2.,9.55,5.));
#10923=CARTESIAN_POINT('Origin',(2.,9.2,5.));
#10924=CARTESIAN_POINT('',(0.,0.,0.));
#10925=CARTESIAN_POINT('Origin',(-2.,9.2,5.));
#10926=CARTESIAN_POINT('',(-2.505,9.55,5.));
#10927=CARTESIAN_POINT('Origin',(-2.,9.55,5.));
#10928=CARTESIAN_POINT('',(-2.505,9.2,5.));
#10929=CARTESIAN_POINT('',(-2.505,9.2,5.));
#10930=CARTESIAN_POINT('Origin',(-2.,9.2,5.));
#10931=CARTESIAN_POINT('Origin',(-2.,9.2,5.));
#10932=CARTESIAN_POINT('',(-2.7,9.55,5.));
#10933=CARTESIAN_POINT('Origin',(-2.,9.55,5.));
#10934=CARTESIAN_POINT('',(-2.7,9.2,5.));
#10935=CARTESIAN_POINT('',(-2.7,9.2,5.));
#10936=CARTESIAN_POINT('Origin',(-2.,9.2,5.));
#10937=CARTESIAN_POINT('Origin',(-2.,9.55,5.));
#10938=CARTESIAN_POINT('Origin',(-2.,9.2,5.));
#10939=CARTESIAN_POINT('',(-4.,-20.,1.));
#10940=CARTESIAN_POINT('',(4.,-20.,1.));
#10941=CARTESIAN_POINT('',(0.,0.,0.));
#10942=CARTESIAN_POINT('',(-4.,-15.,1.42));
#10943=CARTESIAN_POINT('',(-4.,-15.,2.8));
#10944=CARTESIAN_POINT('',(-4.,-15.,2.9));
#10945=CARTESIAN_POINT('',(-4.,4.,1.42));
#10946=CARTESIAN_POINT('',(-4.,4.,2.8));
#10947=CARTESIAN_POINT('',(-4.,4.,2.9));
#10948=CARTESIAN_POINT('',(-4.,15.,1.42));
#10949=CARTESIAN_POINT('',(-4.,15.,2.8));
#10950=CARTESIAN_POINT('',(-4.,15.,2.9));
#10951=CARTESIAN_POINT('',(4.,-15.,1.42));
#10952=CARTESIAN_POINT('',(4.,-15.,2.8));
#10953=CARTESIAN_POINT('',(4.,-15.,2.9));
#10954=CARTESIAN_POINT('',(4.,4.,1.42));
#10955=CARTESIAN_POINT('',(4.,4.,2.8));
#10956=CARTESIAN_POINT('',(4.,4.,2.9));
#10957=CARTESIAN_POINT('',(4.,15.,1.42));
#10958=CARTESIAN_POINT('',(4.,15.,2.8));
#10959=CARTESIAN_POINT('',(4.,15.,2.9));
#10960=CARTESIAN_POINT('',(0.,0.,0.));
#10961=CARTESIAN_POINT('',(0.,0.,0.));
#10962=CARTESIAN_POINT('',(0.,0.,0.));
#10963=CARTESIAN_POINT('',(-3.5,-12.5,3.8));
#10964=CARTESIAN_POINT('',(3.5,-12.5,3.8));
#10965=CARTESIAN_POINT('',(0.,0.,0.));
#10966=CARTESIAN_POINT('',(0.,0.,0.));
#10967=CARTESIAN_POINT('',(0.,0.,0.));
#10968=CARTESIAN_POINT('',(0.,0.,0.));
#10969=CARTESIAN_POINT('',(-2.,-9.,5.));
#10970=CARTESIAN_POINT('',(0.,0.,0.));
#10971=CARTESIAN_POINT('',(0.,0.,0.));
#10972=CARTESIAN_POINT('',(0.,0.,0.));
#10973=CARTESIAN_POINT('',(2.,-9.,5.));
#10974=CARTESIAN_POINT('',(0.,0.,0.));
#10975=CARTESIAN_POINT('',(-3.5,7.5,3.8));
#10976=CARTESIAN_POINT('',(3.5,7.5,3.8));
#10977=CARTESIAN_POINT('',(0.,0.,0.));
#10978=CARTESIAN_POINT('',(0.,0.,0.));
#10979=CARTESIAN_POINT('',(0.,0.,0.));
#10980=CARTESIAN_POINT('',(-2.,11.,5.));
#10981=CARTESIAN_POINT('',(0.,0.,0.));
#10982=CARTESIAN_POINT('',(0.,0.,0.));
#10983=CARTESIAN_POINT('',(0.,0.,0.));
#10984=CARTESIAN_POINT('',(2.,11.,5.));
#10985=CARTESIAN_POINT('',(0.,0.,0.));
#10986=CARTESIAN_POINT('',(5.,-1.2,3.8));
#10987=CARTESIAN_POINT('',(5.,1.2,3.8));
#10988=CARTESIAN_POINT('',(0.,0.,0.));
#10989=CARTESIAN_POINT('',(5.,1.4,12.6));
#10990=CARTESIAN_POINT('',(0.,1.2,12.6));
#10991=CARTESIAN_POINT('',(0.,0.,0.));
#10992=CARTESIAN_POINT('',(0.,0.,0.));
#10993=CARTESIAN_POINT('',(0.,0.,0.));
#10994=CARTESIAN_POINT('',(0.,0.,0.));
#10995=CARTESIAN_POINT('',(0.,0.,0.));
#10996=CARTESIAN_POINT('',(0.,0.,0.));
#10997=CARTESIAN_POINT('',(0.,0.,0.));
#10998=CARTESIAN_POINT('',(0.,0.,0.));
#10999=CARTESIAN_POINT('',(0.,0.,0.));
#11000=CARTESIAN_POINT('Origin',(0.,-16.,6.95959179422654));
#11001=CARTESIAN_POINT('',(-1.,16.,6.95959179422654));
#11002=CARTESIAN_POINT('Origin',(0.,16.,6.95959179422654));
#11003=CARTESIAN_POINT('',(-1.,-16.,6.95959179422654));
#11004=CARTESIAN_POINT('',(-1.,-16.,6.95959179422654));
#11005=CARTESIAN_POINT('Origin',(0.,-16.,6.95959179422654));
#11006=CARTESIAN_POINT('Origin',(0.,16.,6.95959179422654));
#11007=CARTESIAN_POINT('Origin',(0.,-16.,6.95959179422654));
#11008=CARTESIAN_POINT('',(0.,0.,0.));
#11009=CARTESIAN_POINT('',(0.,0.,0.));
#11010=CARTESIAN_POINT('',(0.,0.,0.));
#11011=CARTESIAN_POINT('',(0.,0.,0.));
#11012=CARTESIAN_POINT('Origin',(0.,0.,0.));
#11013=CARTESIAN_POINT('',(-0.976185,-0.246528389340863,-1.19548183562566E-16));
#11014=CARTESIAN_POINT('',(-1.19548183562566E-16,-0.246528389340863,0.976185));
#11015=CARTESIAN_POINT('Origin',(0.,-0.246528389340863,0.));
#11016=CARTESIAN_POINT('Origin',(0.,-0.246528389340863,0.));
#11017=CARTESIAN_POINT('',(-1.19548183562566E-16,0.246528389340863,0.976185));
#11018=CARTESIAN_POINT('Origin',(-1.22464679914735E-16,0.,1.));
#11019=CARTESIAN_POINT('',(-0.976185,0.246528389340863,1.19548183562566E-16));
#11020=CARTESIAN_POINT('Origin',(0.,0.246528389340863,0.));
#11021=CARTESIAN_POINT('Origin',(0.,0.246528389340863,0.));
#11022=CARTESIAN_POINT('Origin',(0.,0.,0.));
#11023=CARTESIAN_POINT('',(-0.976185,0.45,-1.19548183562566E-16));
#11024=CARTESIAN_POINT('',(-0.976185,0.,-1.19548183562566E-16));
#11025=CARTESIAN_POINT('Origin',(0.,0.45,0.));
#11026=CARTESIAN_POINT('Origin',(0.,0.,0.));
#11027=CARTESIAN_POINT('',(-0.5,-0.39,-6.12323399573677E-17));
#11028=CARTESIAN_POINT('Origin',(0.,-0.39,0.));
#11029=CARTESIAN_POINT('',(-0.5,0.39,-6.12323399573677E-17));
#11030=CARTESIAN_POINT('',(-0.5,0.,-6.12323399573677E-17));
#11031=CARTESIAN_POINT('Origin',(0.,0.39,0.));
#11032=CARTESIAN_POINT('Origin',(0.,0.42,0.));
#11033=CARTESIAN_POINT('',(-0.56,0.45,-6.85802207522518E-17));
#11034=CARTESIAN_POINT('',(-0.53,0.42,-6.49062803548097E-17));
#11035=CARTESIAN_POINT('Origin',(0.,0.45,0.));
#11036=CARTESIAN_POINT('Origin',(0.976185,0.45,0.));
#11037=CARTESIAN_POINT('Origin',(0.,0.,0.));
#11038=CARTESIAN_POINT('',(-0.976185,-0.45,-1.19548183562566E-16));
#11039=CARTESIAN_POINT('Origin',(0.,-0.45,0.));
#11040=CARTESIAN_POINT('',(-0.976185,0.,-1.19548183562566E-16));
#11041=CARTESIAN_POINT('Origin',(0.56,-0.45,0.));
#11042=CARTESIAN_POINT('',(-0.56,-0.45,-6.85802207522518E-17));
#11043=CARTESIAN_POINT('Origin',(0.,-0.45,0.));
#11044=CARTESIAN_POINT('Origin',(0.,-0.42,0.));
#11045=CARTESIAN_POINT('',(-0.53,-0.42,-6.49062803548097E-17));
#11046=CARTESIAN_POINT('',(0.,0.,0.));
#11047=CARTESIAN_POINT('Origin',(0.,0.,0.));
#11048=CARTESIAN_POINT('',(-1.023815,0.246528389340863,-1.25381176266905E-16));
#11049=CARTESIAN_POINT('',(-1.25381176266905E-16,0.246528389340863,1.023815));
#11050=CARTESIAN_POINT('Origin',(0.,0.246528389340863,0.));
#11051=CARTESIAN_POINT('Origin',(0.,0.246528389340863,0.));
#11052=CARTESIAN_POINT('',(-1.25381176266905E-16,-0.246528389340863,1.023815));
#11053=CARTESIAN_POINT('Origin',(-1.22464679914735E-16,0.,1.));
#11054=CARTESIAN_POINT('',(-1.023815,-0.246528389340863,1.25381176266905E-16));
#11055=CARTESIAN_POINT('Origin',(0.,-0.246528389340863,0.));
#11056=CARTESIAN_POINT('Origin',(0.,-0.246528389340863,0.));
#11057=CARTESIAN_POINT('Origin',(0.,0.,0.));
#11058=CARTESIAN_POINT('',(-1.023815,-0.45,-1.25381176266905E-16));
#11059=CARTESIAN_POINT('Origin',(0.,-0.45,0.));
#11060=CARTESIAN_POINT('',(-1.023815,0.,-1.25381176266905E-16));
#11061=CARTESIAN_POINT('Origin',(1.44,0.45,0.));
#11062=CARTESIAN_POINT('',(-1.44,0.45,-1.76349139077219E-16));
#11063=CARTESIAN_POINT('Origin',(0.,0.45,0.));
#11064=CARTESIAN_POINT('',(-1.023815,0.45,-1.25381176266905E-16));
#11065=CARTESIAN_POINT('Origin',(0.,0.45,0.));
#11066=CARTESIAN_POINT('Origin',(0.,0.42,0.));
#11067=CARTESIAN_POINT('',(-1.5,0.39,-1.83697019872103E-16));
#11068=CARTESIAN_POINT('Origin',(0.,0.39,0.));
#11069=CARTESIAN_POINT('',(-1.47,0.42,-1.80023079474661E-16));
#11070=CARTESIAN_POINT('Origin',(0.,0.,0.));
#11071=CARTESIAN_POINT('',(-1.5,-0.39,-1.83697019872103E-16));
#11072=CARTESIAN_POINT('Origin',(0.,-0.39,0.));
#11073=CARTESIAN_POINT('',(-1.5,0.,-1.83697019872103E-16));
#11074=CARTESIAN_POINT('Origin',(0.,-0.42,0.));
#11075=CARTESIAN_POINT('',(-1.44,-0.45,-1.76349139077219E-16));
#11076=CARTESIAN_POINT('Origin',(0.,-0.45,0.));
#11077=CARTESIAN_POINT('',(-1.47,-0.42,-1.80023079474661E-16));
#11078=CARTESIAN_POINT('Origin',(1.023815,-0.45,0.));
#11079=CARTESIAN_POINT('Origin',(0.,0.,0.));
#11080=CARTESIAN_POINT('',(-1.023815,0.,-1.25381176266905E-16));
#11081=CARTESIAN_POINT('',(0.,0.,0.));
#11082=CARTESIAN_POINT('Origin',(1.,0.,0.));
#11083=CARTESIAN_POINT('',(1.,-1.78583896120461E-33,0.23815));
#11084=CARTESIAN_POINT('',(1.,-1.78583896120461E-33,-0.23815));
#11085=CARTESIAN_POINT('Origin',(1.,0.,0.));
#11086=CARTESIAN_POINT('Origin',(0.707106781186548,0.,-0.707106781186547));
#11087=CARTESIAN_POINT('',(0.875504261126124,-1.78583896120461E-33,-0.538709301246971));
#11088=CARTESIAN_POINT('',(0.538709301246971,-1.78583896120461E-33,-0.875504261126124));
#11089=CARTESIAN_POINT('Origin',(0.707106781186548,0.,-0.707106781186547));
#11090=CARTESIAN_POINT('Origin',(6.12323399573677E-17,0.,-1.));
#11091=CARTESIAN_POINT('',(0.23815,-1.78583896120461E-33,-1.));
#11092=CARTESIAN_POINT('',(-0.23815,-1.78583896120461E-33,-1.));
#11093=CARTESIAN_POINT('Origin',(6.12323399573677E-17,0.,-1.));
#11094=CARTESIAN_POINT('Origin',(-0.707106781186547,0.,-0.707106781186548));
#11095=CARTESIAN_POINT('',(-0.538709301246971,-1.78583896120461E-33,-0.875504261126124));
#11096=CARTESIAN_POINT('',(-0.875504261126124,-1.78583896120461E-33,-0.538709301246971));
#11097=CARTESIAN_POINT('Origin',(-0.707106781186547,0.,-0.707106781186548));
#11098=CARTESIAN_POINT('Origin',(-1.,0.,-1.22464679914735E-16));
#11099=CARTESIAN_POINT('',(-1.,-1.78583896120461E-33,-0.23815));
#11100=CARTESIAN_POINT('',(-1.,-1.78583896120461E-33,0.23815));
#11101=CARTESIAN_POINT('Origin',(-1.,0.,-1.22464679914735E-16));
#11102=CARTESIAN_POINT('Origin',(-0.707106781186548,0.,0.707106781186547));
#11103=CARTESIAN_POINT('',(-0.875504261126124,-7.94881478324376E-33,0.538709301246971));
#11104=CARTESIAN_POINT('',(-0.538709301246971,4.37713686083455E-33,0.875504261126124));
#11105=CARTESIAN_POINT('Origin',(-0.707106781186548,0.,0.707106781186547));
#11106=CARTESIAN_POINT('Origin',(-1.83697019872103E-16,0.,1.));
#11107=CARTESIAN_POINT('',(-0.23815,-1.78583896120461E-33,1.));
#11108=CARTESIAN_POINT('',(0.23815,-1.78583896120461E-33,1.));
#11109=CARTESIAN_POINT('Origin',(-1.83697019872103E-16,0.,1.));
#11110=CARTESIAN_POINT('Origin',(0.707106781186547,0.,0.707106781186548));
#11111=CARTESIAN_POINT('',(0.538709301246971,-4.86732687222419E-33,0.875504261126124));
#11112=CARTESIAN_POINT('',(0.875504261126124,1.29564894981497E-33,0.538709301246971));
#11113=CARTESIAN_POINT('Origin',(0.707106781186547,0.,0.707106781186548));
#11114=CARTESIAN_POINT('',(0.,0.,0.));
#11115=CARTESIAN_POINT('Origin',(0.707106781186547,0.,0.707106781186548));
#11116=CARTESIAN_POINT('',(0.504455939115715,-0.04763,0.841298510752802));
#11117=CARTESIAN_POINT('',(0.841298510752802,-0.04763,0.504455939115715));
#11118=CARTESIAN_POINT('Ctrl Pts',(0.504455939115715,-0.04763,0.841298510752802));
#11119=CARTESIAN_POINT('Ctrl Pts',(0.508899795931835,-0.0740444353928835,
0.838633903678357));
#11120=CARTESIAN_POINT('Ctrl Pts',(0.517157748491652,-0.0999305678883309,
0.833661031856294));
#11121=CARTESIAN_POINT('Ctrl Pts',(0.537715343527944,-0.142345102874864,
0.820511285096538));
#11122=CARTESIAN_POINT('Ctrl Pts',(0.548874290046456,-0.159766064500479,
0.813159949759));
#11123=CARTESIAN_POINT('Ctrl Pts',(0.573915184558107,-0.190326085855194,
0.795684265985089));
#11124=CARTESIAN_POINT('Ctrl Pts',(0.587792702767295,-0.203463743702801,
0.78555112003688));
#11125=CARTESIAN_POINT('Ctrl Pts',(0.615966552324775,-0.224161999508995,
0.763642258217233));
#11126=CARTESIAN_POINT('Ctrl Pts',(0.631684198665438,-0.232861760990032,
0.750785745543687));
#11127=CARTESIAN_POINT('Ctrl Pts',(0.663382628119203,-0.244251601209411,
0.722929908501543));
#11128=CARTESIAN_POINT('Ctrl Pts',(0.679352081686668,-0.246942143572133,
0.707917883896095));
#11129=CARTESIAN_POINT('Ctrl Pts',(0.707917883896095,-0.246942143572133,
0.679352081686668));
#11130=CARTESIAN_POINT('Ctrl Pts',(0.722929908501543,-0.244251601209411,
0.663382628119203));
#11131=CARTESIAN_POINT('Ctrl Pts',(0.750785745543687,-0.232861760990032,
0.631684198665439));
#11132=CARTESIAN_POINT('Ctrl Pts',(0.763642258217232,-0.224161999508995,
0.615966552324775));
#11133=CARTESIAN_POINT('Ctrl Pts',(0.78555112003688,-0.203463743702801,
0.587792702767295));
#11134=CARTESIAN_POINT('Ctrl Pts',(0.795684265985088,-0.190326085855194,
0.573915184558108));
#11135=CARTESIAN_POINT('Ctrl Pts',(0.813159949759,-0.15976606450048,0.548874290046456));
#11136=CARTESIAN_POINT('Ctrl Pts',(0.820511285096538,-0.142345102874864,
0.537715343527944));
#11137=CARTESIAN_POINT('Ctrl Pts',(0.833661031856294,-0.099930567888331,
0.517157748491653));
#11138=CARTESIAN_POINT('Ctrl Pts',(0.838633903678357,-0.0740444353928835,
0.508899795931835));
#11139=CARTESIAN_POINT('Ctrl Pts',(0.841298510752801,-0.0476299999999999,
0.504455939115715));
#11140=CARTESIAN_POINT('',(0.528110872004958,-0.04763,0.871530771444223));
#11141=CARTESIAN_POINT('Origin',(0.707106781186547,-0.04763,0.707106781186548));
#11142=CARTESIAN_POINT('',(0.871530771444223,-0.04763,0.528110872004959));
#11143=CARTESIAN_POINT('Ctrl Pts',(0.871530771444223,-0.0476300000000001,
0.528110872004958));
#11144=CARTESIAN_POINT('Ctrl Pts',(0.87014664509073,-0.0609922781173483,
0.530395067942936));
#11145=CARTESIAN_POINT('Ctrl Pts',(0.868149331745851,-0.0742967091364493,
0.533674141594226));
#11146=CARTESIAN_POINT('Ctrl Pts',(0.85981294420286,-0.115492077056649,
0.54708917182331));
#11147=CARTESIAN_POINT('Ctrl Pts',(0.850993704737257,-0.141695629206859,
0.560922177770136));
#11148=CARTESIAN_POINT('Ctrl Pts',(0.830754510485543,-0.181890537957859,
0.590422647829571));
#11149=CARTESIAN_POINT('Ctrl Pts',(0.816896541396381,-0.201072148666545,
0.609616703125488));
#11150=CARTESIAN_POINT('Ctrl Pts',(0.792310597819928,-0.223955109275652,
0.641117951819998));
#11151=CARTESIAN_POINT('Ctrl Pts',(0.779109323683612,-0.232742381310829,
0.657208095763053));
#11152=CARTESIAN_POINT('Ctrl Pts',(0.750552691816206,-0.244234834628584,
0.68964083160521));
#11153=CARTESIAN_POINT('Ctrl Pts',(0.735185187071673,-0.246942143572133,
0.705971972091755));
#11154=CARTESIAN_POINT('Ctrl Pts',(0.705971972091754,-0.246942143572133,
0.735185187071673));
#11155=CARTESIAN_POINT('Ctrl Pts',(0.689640831605209,-0.244234834628584,
0.750552691816206));
#11156=CARTESIAN_POINT('Ctrl Pts',(0.657208095763052,-0.232742381310829,
0.779109323683612));
#11157=CARTESIAN_POINT('Ctrl Pts',(0.641117951819998,-0.223955109275652,
0.792310597819928));
#11158=CARTESIAN_POINT('Ctrl Pts',(0.609616703125487,-0.201072148666545,
0.816896541396382));
#11159=CARTESIAN_POINT('Ctrl Pts',(0.590422647829571,-0.181890537957858,
0.830754510485544));
#11160=CARTESIAN_POINT('Ctrl Pts',(0.560922177770135,-0.141695629206858,
0.850993704737257));
#11161=CARTESIAN_POINT('Ctrl Pts',(0.547089171823309,-0.115492077056649,
0.859812944202861));
#11162=CARTESIAN_POINT('Ctrl Pts',(0.533674141594226,-0.0742967091364491,
0.868149331745852));
#11163=CARTESIAN_POINT('Ctrl Pts',(0.530395067942936,-0.0609922781173483,
0.870146645090731));
#11164=CARTESIAN_POINT('Ctrl Pts',(0.528110872004958,-0.0476300000000001,
0.871530771444223));
#11165=CARTESIAN_POINT('Origin',(0.707106781186547,-0.04763,0.707106781186548));
#11166=CARTESIAN_POINT('Origin',(0.,-0.166705,0.));
#11167=CARTESIAN_POINT('',(0.242834539687906,-0.04763,0.989696097314));
#11168=CARTESIAN_POINT('Origin',(0.,-0.04763,0.));
#11169=CARTESIAN_POINT('',(-0.242834539687907,-0.04763,0.989696097314));
#11170=CARTESIAN_POINT('Ctrl Pts',(0.242834539687906,-0.04763,0.989696097314));
#11171=CARTESIAN_POINT('Ctrl Pts',(0.24024064412003,-0.0609922781173483,
0.990332542620729));
#11172=CARTESIAN_POINT('Ctrl Pts',(0.236509675094874,-0.0742967091364492,
0.991238884025248));
#11173=CARTESIAN_POINT('Ctrl Pts',(0.221129100087819,-0.115492077056649,
0.994830026707808));
#11174=CARTESIAN_POINT('Ctrl Pts',(0.205111543747588,-0.141695629206859,
0.998375294985966));
#11175=CARTESIAN_POINT('Ctrl Pts',(0.169940289819232,-0.181890537957859,
1.00492400591205));
#11176=CARTESIAN_POINT('Ctrl Pts',(0.1465689792446,-0.201072148666545,1.00869718865384));
#11177=CARTESIAN_POINT('Ctrl Pts',(0.106909345252087,-0.223955109275652,
1.01358704779679));
#11178=CARTESIAN_POINT('Ctrl Pts',(0.0861971848975941,-0.232742381310829,
1.0156297872271));
#11179=CARTESIAN_POINT('Ctrl Pts',(0.0430711894098822,-0.244234834628584,
1.01837060663223));
#11180=CARTESIAN_POINT('Ctrl Pts',(0.0206568624125605,-0.246942143572133,
1.019052));
#11181=CARTESIAN_POINT('Ctrl Pts',(-0.0206568624125608,-0.246942143572133,
1.019052));
#11182=CARTESIAN_POINT('Ctrl Pts',(-0.0430711894098825,-0.244234834628584,
1.01837060663223));
#11183=CARTESIAN_POINT('Ctrl Pts',(-0.0861971848975943,-0.232742381310829,
1.0156297872271));
#11184=CARTESIAN_POINT('Ctrl Pts',(-0.106909345252088,-0.223955109275652,
1.01358704779679));
#11185=CARTESIAN_POINT('Ctrl Pts',(-0.1465689792446,-0.201072148666545,
1.00869718865384));
#11186=CARTESIAN_POINT('Ctrl Pts',(-0.169940289819232,-0.181890537957859,
1.00492400591205));
#11187=CARTESIAN_POINT('Ctrl Pts',(-0.205111543747588,-0.141695629206859,
0.998375294985966));
#11188=CARTESIAN_POINT('Ctrl Pts',(-0.221129100087819,-0.115492077056649,
0.994830026707808));
#11189=CARTESIAN_POINT('Ctrl Pts',(-0.236509675094875,-0.0742967091364493,
0.991238884025248));
#11190=CARTESIAN_POINT('Ctrl Pts',(-0.24024064412003,-0.0609922781173483,
0.990332542620729));
#11191=CARTESIAN_POINT('Ctrl Pts',(-0.242834539687907,-0.04763,0.989696097314));
#11192=CARTESIAN_POINT('',(-0.528110872004959,-0.04763,0.871530771444223));
#11193=CARTESIAN_POINT('Origin',(0.,-0.04763,0.));
#11194=CARTESIAN_POINT('',(-0.871530771444223,-0.04763,0.528110872004958));
#11195=CARTESIAN_POINT('Ctrl Pts',(-0.528110872004958,-0.0476300000000001,
0.871530771444223));
#11196=CARTESIAN_POINT('Ctrl Pts',(-0.530395067942936,-0.0609922781173484,
0.87014664509073));
#11197=CARTESIAN_POINT('Ctrl Pts',(-0.533674141594226,-0.0742967091364493,
0.868149331745851));
#11198=CARTESIAN_POINT('Ctrl Pts',(-0.54708917182331,-0.115492077056649,
0.85981294420286));
#11199=CARTESIAN_POINT('Ctrl Pts',(-0.560922177770136,-0.141695629206859,
0.850993704737257));
#11200=CARTESIAN_POINT('Ctrl Pts',(-0.590422647829571,-0.181890537957859,
0.830754510485543));
#11201=CARTESIAN_POINT('Ctrl Pts',(-0.609616703125488,-0.201072148666545,
0.816896541396381));
#11202=CARTESIAN_POINT('Ctrl Pts',(-0.641117951819998,-0.223955109275652,
0.792310597819928));
#11203=CARTESIAN_POINT('Ctrl Pts',(-0.657208095763053,-0.232742381310829,
0.779109323683611));
#11204=CARTESIAN_POINT('Ctrl Pts',(-0.68964083160521,-0.244234834628584,
0.750552691816205));
#11205=CARTESIAN_POINT('Ctrl Pts',(-0.705971972091755,-0.246942143572133,
0.735185187071673));
#11206=CARTESIAN_POINT('Ctrl Pts',(-0.735185187071673,-0.246942143572133,
0.705971972091754));
#11207=CARTESIAN_POINT('Ctrl Pts',(-0.750552691816206,-0.244234834628584,
0.689640831605209));
#11208=CARTESIAN_POINT('Ctrl Pts',(-0.779109323683612,-0.232742381310829,
0.657208095763052));
#11209=CARTESIAN_POINT('Ctrl Pts',(-0.792310597819928,-0.223955109275652,
0.641117951819998));
#11210=CARTESIAN_POINT('Ctrl Pts',(-0.816896541396382,-0.201072148666545,
0.609616703125487));
#11211=CARTESIAN_POINT('Ctrl Pts',(-0.830754510485544,-0.181890537957858,
0.590422647829571));
#11212=CARTESIAN_POINT('Ctrl Pts',(-0.850993704737257,-0.141695629206858,
0.560922177770135));
#11213=CARTESIAN_POINT('Ctrl Pts',(-0.859812944202861,-0.115492077056649,
0.547089171823309));
#11214=CARTESIAN_POINT('Ctrl Pts',(-0.868149331745852,-0.0742967091364491,
0.533674141594226));
#11215=CARTESIAN_POINT('Ctrl Pts',(-0.870146645090731,-0.0609922781173483,
0.530395067942936));
#11216=CARTESIAN_POINT('Ctrl Pts',(-0.871530771444223,-0.04763,0.528110872004958));
#11217=CARTESIAN_POINT('',(-0.989696097314,-0.04763,0.242834539687906));
#11218=CARTESIAN_POINT('Origin',(0.,-0.04763,0.));
#11219=CARTESIAN_POINT('',(-1.019052,-0.246942143572133,1.248489836334E-16));
#11220=CARTESIAN_POINT('Ctrl Pts',(-0.989696097314,-0.04763,0.242834539687906));
#11221=CARTESIAN_POINT('Ctrl Pts',(-0.990332542620729,-0.0609922781173483,
0.24024064412003));
#11222=CARTESIAN_POINT('Ctrl Pts',(-0.991238884025248,-0.0742967091364492,
0.236509675094874));
#11223=CARTESIAN_POINT('Ctrl Pts',(-0.994830026707808,-0.115492077056649,
0.221129100087819));
#11224=CARTESIAN_POINT('Ctrl Pts',(-0.998375294985966,-0.141695629206859,
0.205111543747588));
#11225=CARTESIAN_POINT('Ctrl Pts',(-1.00492400591205,-0.181890537957859,
0.169940289819232));
#11226=CARTESIAN_POINT('Ctrl Pts',(-1.00869718865384,-0.201072148666545,
0.1465689792446));
#11227=CARTESIAN_POINT('Ctrl Pts',(-1.01358704779679,-0.223955109275652,
0.106909345252088));
#11228=CARTESIAN_POINT('Ctrl Pts',(-1.0156297872271,-0.232742381310829,
0.0861971848975944));
#11229=CARTESIAN_POINT('Ctrl Pts',(-1.01837060663223,-0.244234834628584,
0.0430711894098825));
#11230=CARTESIAN_POINT('Ctrl Pts',(-1.019052,-0.246942143572133,0.0206568624125608));
#11231=CARTESIAN_POINT('Ctrl Pts',(-1.019052,-0.246942143572133,1.2490009027033E-16));
#11232=CARTESIAN_POINT('',(-1.019052,-0.28578,1.24797876996471E-16));
#11233=CARTESIAN_POINT('',(-1.019052,-0.166705,1.24797876996471E-16));
#11234=CARTESIAN_POINT('Origin',(0.,-0.28578,0.));
#11235=CARTESIAN_POINT('',(-0.989696097314,-0.04763,-0.242834539687906));
#11236=CARTESIAN_POINT('Ctrl Pts',(-1.019052,-0.246942143572133,1.2490009027033E-16));
#11237=CARTESIAN_POINT('Ctrl Pts',(-1.019052,-0.246942143572133,-0.0206568624125605));
#11238=CARTESIAN_POINT('Ctrl Pts',(-1.01837060663223,-0.244234834628584,
-0.0430711894098822));
#11239=CARTESIAN_POINT('Ctrl Pts',(-1.0156297872271,-0.232742381310829,
-0.0861971848975941));
#11240=CARTESIAN_POINT('Ctrl Pts',(-1.01358704779679,-0.223955109275652,
-0.106909345252087));
#11241=CARTESIAN_POINT('Ctrl Pts',(-1.00869718865384,-0.201072148666546,
-0.1465689792446));
#11242=CARTESIAN_POINT('Ctrl Pts',(-1.00492400591205,-0.181890537957859,
-0.169940289819232));
#11243=CARTESIAN_POINT('Ctrl Pts',(-0.998375294985966,-0.141695629206859,
-0.205111543747588));
#11244=CARTESIAN_POINT('Ctrl Pts',(-0.994830026707808,-0.11549207705665,
-0.221129100087819));
#11245=CARTESIAN_POINT('Ctrl Pts',(-0.991238884025248,-0.0742967091364495,
-0.236509675094874));
#11246=CARTESIAN_POINT('Ctrl Pts',(-0.990332542620729,-0.0609922781173484,
-0.24024064412003));
#11247=CARTESIAN_POINT('Ctrl Pts',(-0.989696097314,-0.0476300000000001,
-0.242834539687907));
#11248=CARTESIAN_POINT('',(-0.871530771444223,-0.04763,-0.528110872004958));
#11249=CARTESIAN_POINT('Origin',(0.,-0.04763,0.));
#11250=CARTESIAN_POINT('',(-0.528110872004958,-0.04763,-0.871530771444223));
#11251=CARTESIAN_POINT('Ctrl Pts',(-0.871530771444223,-0.0476300000000001,
-0.528110872004958));
#11252=CARTESIAN_POINT('Ctrl Pts',(-0.87014664509073,-0.0609922781173484,
-0.530395067942936));
#11253=CARTESIAN_POINT('Ctrl Pts',(-0.868149331745851,-0.0742967091364494,
-0.533674141594226));
#11254=CARTESIAN_POINT('Ctrl Pts',(-0.85981294420286,-0.115492077056649,
-0.54708917182331));
#11255=CARTESIAN_POINT('Ctrl Pts',(-0.850993704737257,-0.141695629206859,
-0.560922177770136));
#11256=CARTESIAN_POINT('Ctrl Pts',(-0.830754510485543,-0.181890537957859,
-0.590422647829571));
#11257=CARTESIAN_POINT('Ctrl Pts',(-0.816896541396381,-0.201072148666546,
-0.609616703125488));
#11258=CARTESIAN_POINT('Ctrl Pts',(-0.792310597819928,-0.223955109275652,
-0.641117951819999));
#11259=CARTESIAN_POINT('Ctrl Pts',(-0.779109323683611,-0.232742381310829,
-0.657208095763053));
#11260=CARTESIAN_POINT('Ctrl Pts',(-0.750552691816205,-0.244234834628584,
-0.68964083160521));
#11261=CARTESIAN_POINT('Ctrl Pts',(-0.735185187071673,-0.246942143572133,
-0.705971972091755));
#11262=CARTESIAN_POINT('Ctrl Pts',(-0.705971972091754,-0.246942143572133,
-0.735185187071673));
#11263=CARTESIAN_POINT('Ctrl Pts',(-0.68964083160521,-0.244234834628584,
-0.750552691816206));
#11264=CARTESIAN_POINT('Ctrl Pts',(-0.657208095763052,-0.232742381310829,
-0.779109323683612));
#11265=CARTESIAN_POINT('Ctrl Pts',(-0.641117951819998,-0.223955109275652,
-0.792310597819928));
#11266=CARTESIAN_POINT('Ctrl Pts',(-0.609616703125488,-0.201072148666545,
-0.816896541396381));
#11267=CARTESIAN_POINT('Ctrl Pts',(-0.590422647829571,-0.181890537957859,
-0.830754510485543));
#11268=CARTESIAN_POINT('Ctrl Pts',(-0.560922177770136,-0.141695629206859,
-0.850993704737257));
#11269=CARTESIAN_POINT('Ctrl Pts',(-0.54708917182331,-0.115492077056649,
-0.85981294420286));
#11270=CARTESIAN_POINT('Ctrl Pts',(-0.533674141594226,-0.0742967091364494,
-0.868149331745852));
#11271=CARTESIAN_POINT('Ctrl Pts',(-0.530395067942936,-0.0609922781173484,
-0.870146645090731));
#11272=CARTESIAN_POINT('Ctrl Pts',(-0.528110872004958,-0.0476300000000001,
-0.871530771444223));
#11273=CARTESIAN_POINT('',(-0.242834539687906,-0.04763,-0.989696097314));
#11274=CARTESIAN_POINT('Origin',(0.,-0.04763,0.));
#11275=CARTESIAN_POINT('',(0.242834539687906,-0.04763,-0.989696097314));
#11276=CARTESIAN_POINT('Ctrl Pts',(-0.242834539687907,-0.04763,-0.989696097314));
#11277=CARTESIAN_POINT('Ctrl Pts',(-0.24024064412003,-0.0609922781173483,
-0.990332542620729));
#11278=CARTESIAN_POINT('Ctrl Pts',(-0.236509675094874,-0.0742967091364493,
-0.991238884025248));
#11279=CARTESIAN_POINT('Ctrl Pts',(-0.221129100087819,-0.115492077056649,
-0.994830026707808));
#11280=CARTESIAN_POINT('Ctrl Pts',(-0.205111543747588,-0.141695629206859,
-0.998375294985966));
#11281=CARTESIAN_POINT('Ctrl Pts',(-0.169940289819232,-0.181890537957859,
-1.00492400591205));
#11282=CARTESIAN_POINT('Ctrl Pts',(-0.1465689792446,-0.201072148666545,
-1.00869718865384));
#11283=CARTESIAN_POINT('Ctrl Pts',(-0.106909345252087,-0.223955109275652,
-1.01358704779679));
#11284=CARTESIAN_POINT('Ctrl Pts',(-0.0861971848975942,-0.232742381310829,
-1.0156297872271));
#11285=CARTESIAN_POINT('Ctrl Pts',(-0.0430711894098823,-0.244234834628584,
-1.01837060663223));
#11286=CARTESIAN_POINT('Ctrl Pts',(-0.0206568624125606,-0.246942143572133,
-1.019052));
#11287=CARTESIAN_POINT('Ctrl Pts',(0.0206568624125607,-0.246942143572133,
-1.019052));
#11288=CARTESIAN_POINT('Ctrl Pts',(0.0430711894098824,-0.244234834628584,
-1.01837060663223));
#11289=CARTESIAN_POINT('Ctrl Pts',(0.0861971848975943,-0.232742381310829,
-1.0156297872271));
#11290=CARTESIAN_POINT('Ctrl Pts',(0.106909345252088,-0.223955109275652,
-1.01358704779679));
#11291=CARTESIAN_POINT('Ctrl Pts',(0.1465689792446,-0.201072148666545,-1.00869718865384));
#11292=CARTESIAN_POINT('Ctrl Pts',(0.169940289819232,-0.181890537957859,
-1.00492400591205));
#11293=CARTESIAN_POINT('Ctrl Pts',(0.205111543747588,-0.141695629206859,
-0.998375294985966));
#11294=CARTESIAN_POINT('Ctrl Pts',(0.221129100087819,-0.115492077056649,
-0.994830026707808));
#11295=CARTESIAN_POINT('Ctrl Pts',(0.236509675094874,-0.0742967091364493,
-0.991238884025248));
#11296=CARTESIAN_POINT('Ctrl Pts',(0.24024064412003,-0.0609922781173484,
-0.990332542620729));
#11297=CARTESIAN_POINT('Ctrl Pts',(0.242834539687907,-0.04763,-0.989696097314));
#11298=CARTESIAN_POINT('',(0.528110872004958,-0.04763,-0.871530771444223));
#11299=CARTESIAN_POINT('Origin',(0.,-0.04763,0.));
#11300=CARTESIAN_POINT('',(0.871530771444223,-0.04763,-0.528110872004958));
#11301=CARTESIAN_POINT('Ctrl Pts',(0.528110872004958,-0.0476300000000001,
-0.871530771444223));
#11302=CARTESIAN_POINT('Ctrl Pts',(0.530395067942936,-0.0609922781173484,
-0.870146645090731));
#11303=CARTESIAN_POINT('Ctrl Pts',(0.533674141594226,-0.0742967091364493,
-0.868149331745851));
#11304=CARTESIAN_POINT('Ctrl Pts',(0.54708917182331,-0.115492077056649,
-0.85981294420286));
#11305=CARTESIAN_POINT('Ctrl Pts',(0.560922177770136,-0.141695629206859,
-0.850993704737257));
#11306=CARTESIAN_POINT('Ctrl Pts',(0.590422647829571,-0.181890537957859,
-0.830754510485543));
#11307=CARTESIAN_POINT('Ctrl Pts',(0.609616703125488,-0.201072148666545,
-0.816896541396381));
#11308=CARTESIAN_POINT('Ctrl Pts',(0.641117951819998,-0.223955109275652,
-0.792310597819928));
#11309=CARTESIAN_POINT('Ctrl Pts',(0.657208095763053,-0.232742381310829,
-0.779109323683612));
#11310=CARTESIAN_POINT('Ctrl Pts',(0.68964083160521,-0.244234834628584,
-0.750552691816206));
#11311=CARTESIAN_POINT('Ctrl Pts',(0.705971972091755,-0.246942143572133,
-0.735185187071673));
#11312=CARTESIAN_POINT('Ctrl Pts',(0.735185187071673,-0.246942143572133,
-0.705971972091754));
#11313=CARTESIAN_POINT('Ctrl Pts',(0.750552691816206,-0.244234834628584,
-0.68964083160521));
#11314=CARTESIAN_POINT('Ctrl Pts',(0.779109323683612,-0.232742381310829,
-0.657208095763053));
#11315=CARTESIAN_POINT('Ctrl Pts',(0.792310597819928,-0.223955109275652,
-0.641117951819998));
#11316=CARTESIAN_POINT('Ctrl Pts',(0.816896541396381,-0.201072148666545,
-0.609616703125488));
#11317=CARTESIAN_POINT('Ctrl Pts',(0.830754510485543,-0.181890537957859,
-0.590422647829571));
#11318=CARTESIAN_POINT('Ctrl Pts',(0.850993704737257,-0.141695629206859,
-0.560922177770136));
#11319=CARTESIAN_POINT('Ctrl Pts',(0.85981294420286,-0.115492077056649,
-0.54708917182331));
#11320=CARTESIAN_POINT('Ctrl Pts',(0.868149331745851,-0.0742967091364493,
-0.533674141594226));
#11321=CARTESIAN_POINT('Ctrl Pts',(0.870146645090731,-0.0609922781173484,
-0.530395067942936));
#11322=CARTESIAN_POINT('Ctrl Pts',(0.871530771444223,-0.0476300000000001,
-0.528110872004958));
#11323=CARTESIAN_POINT('',(0.989696097314,-0.04763,-0.242834539687906));
#11324=CARTESIAN_POINT('Origin',(0.,-0.04763,0.));
#11325=CARTESIAN_POINT('',(0.989696097314,-0.04763,0.242834539687906));
#11326=CARTESIAN_POINT('Ctrl Pts',(0.989696097314,-0.04763,-0.242834539687907));
#11327=CARTESIAN_POINT('Ctrl Pts',(0.990332542620729,-0.0609922781173483,
-0.24024064412003));
#11328=CARTESIAN_POINT('Ctrl Pts',(0.991238884025248,-0.0742967091364493,
-0.236509675094874));
#11329=CARTESIAN_POINT('Ctrl Pts',(0.994830026707808,-0.115492077056649,
-0.221129100087819));
#11330=CARTESIAN_POINT('Ctrl Pts',(0.998375294985966,-0.141695629206859,
-0.205111543747588));
#11331=CARTESIAN_POINT('Ctrl Pts',(1.00492400591205,-0.181890537957859,
-0.169940289819232));
#11332=CARTESIAN_POINT('Ctrl Pts',(1.00869718865384,-0.201072148666545,
-0.1465689792446));
#11333=CARTESIAN_POINT('Ctrl Pts',(1.01358704779679,-0.223955109275652,
-0.106909345252087));
#11334=CARTESIAN_POINT('Ctrl Pts',(1.0156297872271,-0.232742381310829,-0.0861971848975942));
#11335=CARTESIAN_POINT('Ctrl Pts',(1.01837060663223,-0.244234834628584,
-0.0430711894098823));
#11336=CARTESIAN_POINT('Ctrl Pts',(1.019052,-0.246942143572133,-0.0206568624125607));
#11337=CARTESIAN_POINT('Ctrl Pts',(1.019052,-0.246942143572133,0.0206568624125607));
#11338=CARTESIAN_POINT('Ctrl Pts',(1.01837060663223,-0.244234834628584,
0.0430711894098823));
#11339=CARTESIAN_POINT('Ctrl Pts',(1.0156297872271,-0.232742381310829,0.0861971848975942));
#11340=CARTESIAN_POINT('Ctrl Pts',(1.01358704779679,-0.223955109275652,
0.106909345252087));
#11341=CARTESIAN_POINT('Ctrl Pts',(1.00869718865384,-0.201072148666545,
0.1465689792446));
#11342=CARTESIAN_POINT('Ctrl Pts',(1.00492400591205,-0.181890537957859,
0.169940289819232));
#11343=CARTESIAN_POINT('Ctrl Pts',(0.998375294985966,-0.141695629206859,
0.205111543747588));
#11344=CARTESIAN_POINT('Ctrl Pts',(0.994830026707808,-0.115492077056649,
0.221129100087819));
#11345=CARTESIAN_POINT('Ctrl Pts',(0.991238884025248,-0.0742967091364492,
0.236509675094874));
#11346=CARTESIAN_POINT('Ctrl Pts',(0.990332542620729,-0.0609922781173483,
0.24024064412003));
#11347=CARTESIAN_POINT('Ctrl Pts',(0.989696097314,-0.04763,0.242834539687907));
#11348=CARTESIAN_POINT('Origin',(0.,-0.04763,0.));
#11349=CARTESIAN_POINT('Origin',(0.,-0.04763,0.));
#11350=CARTESIAN_POINT('',(0.238183666596899,-0.04763,0.951592097314));
#11351=CARTESIAN_POINT('Origin',(0.,-0.04763,0.));
#11352=CARTESIAN_POINT('Origin',(-1.94289029309402E-16,-0.04763,1.));
#11353=CARTESIAN_POINT('Origin',(-1.94289029309402E-16,0.,1.));
#11354=CARTESIAN_POINT('',(-0.2381836665969,-0.04763,0.951592097314));
#11355=CARTESIAN_POINT('Ctrl Pts',(-0.238183666596899,-0.0476299999999999,
0.951592097314));
#11356=CARTESIAN_POINT('Ctrl Pts',(-0.233157223576062,-0.0740444353928835,
0.952850216871763));
#11357=CARTESIAN_POINT('Ctrl Pts',(-0.223801617934946,-0.0999305678883309,
0.955173119738174));
#11358=CARTESIAN_POINT('Ctrl Pts',(-0.199966927975188,-0.142345102874864,
0.960411259488514));
#11359=CARTESIAN_POINT('Ctrl Pts',(-0.1868781821531,-0.159766064500479,
0.963103647174702));
#11360=CARTESIAN_POINT('Ctrl Pts',(-0.15681442133453,-0.190326085855194,
0.968453058988463));
#11361=CARTESIAN_POINT('Ctrl Pts',(-0.139836317888043,-0.203463743702801,
0.971100730005489));
#11362=CARTESIAN_POINT('Ctrl Pts',(-0.104422493053067,-0.224161999508995,
0.975530745318961));
#11363=CARTESIAN_POINT('Ctrl Pts',(-0.0842175114474176,-0.232861760990032,
0.977553872336861));
#11364=CARTESIAN_POINT('Ctrl Pts',(-0.0421062857595701,-0.244251601209411,
0.980270995488453));
#11365=CARTESIAN_POINT('Ctrl Pts',(-0.0201990724523197,-0.246942143572133,
0.980948));
#11366=CARTESIAN_POINT('Ctrl Pts',(0.020199072452319,-0.246942143572133,
0.980948));
#11367=CARTESIAN_POINT('Ctrl Pts',(0.0421062857595694,-0.244251601209411,
0.980270995488454));
#11368=CARTESIAN_POINT('Ctrl Pts',(0.0842175114474169,-0.232861760990032,
0.977553872336861));
#11369=CARTESIAN_POINT('Ctrl Pts',(0.104422493053067,-0.224161999508995,
0.975530745318961));
#11370=CARTESIAN_POINT('Ctrl Pts',(0.139836317888042,-0.203463743702801,
0.971100730005489));
#11371=CARTESIAN_POINT('Ctrl Pts',(0.15681442133453,-0.190326085855194,
0.968453058988463));
#11372=CARTESIAN_POINT('Ctrl Pts',(0.1868781821531,-0.15976606450048,0.963103647174702));
#11373=CARTESIAN_POINT('Ctrl Pts',(0.199966927975188,-0.142345102874864,
0.960411259488514));
#11374=CARTESIAN_POINT('Ctrl Pts',(0.223801617934945,-0.0999305678883309,
0.955173119738174));
#11375=CARTESIAN_POINT('Ctrl Pts',(0.233157223576061,-0.0740444353928835,
0.952850216871763));
#11376=CARTESIAN_POINT('Ctrl Pts',(0.238183666596899,-0.0476299999999999,
0.951592097314));
#11377=CARTESIAN_POINT('Origin',(-1.94289029309402E-16,-0.04763,1.));
#11378=CARTESIAN_POINT('Origin',(0.,-0.04763,0.));
#11379=CARTESIAN_POINT('',(-0.504455939115715,-0.04763,0.841298510752802));
#11380=CARTESIAN_POINT('Origin',(0.,-0.04763,0.));
#11381=CARTESIAN_POINT('Origin',(-0.707106781186548,-0.04763,0.707106781186547));
#11382=CARTESIAN_POINT('Origin',(-0.707106781186548,0.,0.707106781186547));
#11383=CARTESIAN_POINT('',(-0.841298510752802,-0.04763,0.504455939115715));
#11384=CARTESIAN_POINT('Ctrl Pts',(-0.841298510752802,-0.04763,0.504455939115715));
#11385=CARTESIAN_POINT('Ctrl Pts',(-0.838633903678357,-0.0740444353928835,
0.508899795931835));
#11386=CARTESIAN_POINT('Ctrl Pts',(-0.833661031856294,-0.0999305678883309,
0.517157748491652));
#11387=CARTESIAN_POINT('Ctrl Pts',(-0.820511285096538,-0.142345102874864,
0.537715343527944));
#11388=CARTESIAN_POINT('Ctrl Pts',(-0.813159949759,-0.159766064500479,0.548874290046456));
#11389=CARTESIAN_POINT('Ctrl Pts',(-0.795684265985089,-0.190326085855194,
0.573915184558107));
#11390=CARTESIAN_POINT('Ctrl Pts',(-0.78555112003688,-0.203463743702801,
0.587792702767295));
#11391=CARTESIAN_POINT('Ctrl Pts',(-0.763642258217233,-0.224161999508995,
0.615966552324775));
#11392=CARTESIAN_POINT('Ctrl Pts',(-0.750785745543687,-0.232861760990032,
0.631684198665438));
#11393=CARTESIAN_POINT('Ctrl Pts',(-0.722929908501543,-0.244251601209411,
0.663382628119203));
#11394=CARTESIAN_POINT('Ctrl Pts',(-0.707917883896095,-0.246942143572133,
0.679352081686668));
#11395=CARTESIAN_POINT('Ctrl Pts',(-0.679352081686668,-0.246942143572133,
0.707917883896095));
#11396=CARTESIAN_POINT('Ctrl Pts',(-0.663382628119203,-0.244251601209411,
0.722929908501544));
#11397=CARTESIAN_POINT('Ctrl Pts',(-0.631684198665438,-0.232861760990031,
0.750785745543687));
#11398=CARTESIAN_POINT('Ctrl Pts',(-0.615966552324775,-0.224161999508995,
0.763642258217233));
#11399=CARTESIAN_POINT('Ctrl Pts',(-0.587792702767295,-0.203463743702801,
0.78555112003688));
#11400=CARTESIAN_POINT('Ctrl Pts',(-0.573915184558107,-0.190326085855194,
0.795684265985088));
#11401=CARTESIAN_POINT('Ctrl Pts',(-0.548874290046456,-0.159766064500479,
0.813159949759));
#11402=CARTESIAN_POINT('Ctrl Pts',(-0.537715343527944,-0.142345102874864,
0.820511285096538));
#11403=CARTESIAN_POINT('Ctrl Pts',(-0.517157748491652,-0.0999305678883309,
0.833661031856294));
#11404=CARTESIAN_POINT('Ctrl Pts',(-0.508899795931835,-0.0740444353928835,
0.838633903678357));
#11405=CARTESIAN_POINT('Ctrl Pts',(-0.504455939115716,-0.04763,0.841298510752801));
#11406=CARTESIAN_POINT('Origin',(-0.707106781186548,-0.04763,0.707106781186547));
#11407=CARTESIAN_POINT('Origin',(0.,-0.04763,0.));
#11408=CARTESIAN_POINT('',(-0.951592097314,-0.04763,0.238183666596899));
#11409=CARTESIAN_POINT('Origin',(0.,-0.04763,0.));
#11410=CARTESIAN_POINT('Origin',(-1.,-0.04763,-1.11022302462516E-16));
#11411=CARTESIAN_POINT('Origin',(-1.,0.,-1.11022302462516E-16));
#11412=CARTESIAN_POINT('',(-0.951592097314,-0.04763,-0.2381836665969));
#11413=CARTESIAN_POINT('',(-0.980948,-0.246942143572133,1.08514323328844E-18));
#11414=CARTESIAN_POINT('Ctrl Pts',(-0.951592097314,-0.04763,-0.238183666596899));
#11415=CARTESIAN_POINT('Ctrl Pts',(-0.952850216871763,-0.0740444353928835,
-0.233157223576062));
#11416=CARTESIAN_POINT('Ctrl Pts',(-0.955173119738174,-0.0999305678883309,
-0.223801617934946));
#11417=CARTESIAN_POINT('Ctrl Pts',(-0.960411259488514,-0.142345102874864,
-0.199966927975188));
#11418=CARTESIAN_POINT('Ctrl Pts',(-0.963103647174702,-0.159766064500479,
-0.1868781821531));
#11419=CARTESIAN_POINT('Ctrl Pts',(-0.968453058988463,-0.190326085855194,
-0.15681442133453));
#11420=CARTESIAN_POINT('Ctrl Pts',(-0.971100730005489,-0.203463743702801,
-0.139836317888043));
#11421=CARTESIAN_POINT('Ctrl Pts',(-0.975530745318961,-0.224161999508995,
-0.104422493053067));
#11422=CARTESIAN_POINT('Ctrl Pts',(-0.977553872336861,-0.232861760990032,
-0.0842175114474175));
#11423=CARTESIAN_POINT('Ctrl Pts',(-0.980270995488453,-0.244251601209411,
-0.0421062857595699));
#11424=CARTESIAN_POINT('Ctrl Pts',(-0.980948,-0.246942143572133,-0.0201990724523195));
#11425=CARTESIAN_POINT('Ctrl Pts',(-0.980948,-0.246942143572133,-1.17961196366423E-16));
#11426=CARTESIAN_POINT('Origin',(-1.,-0.04763,-1.11022302462516E-16));
#11427=CARTESIAN_POINT('Ctrl Pts',(-0.980948,-0.246942143572133,-1.17961196366423E-16));
#11428=CARTESIAN_POINT('Ctrl Pts',(-0.980948,-0.246942143572133,0.0201990724523192));
#11429=CARTESIAN_POINT('Ctrl Pts',(-0.980270995488453,-0.244251601209411,
0.0421062857595695));
#11430=CARTESIAN_POINT('Ctrl Pts',(-0.977553872336861,-0.232861760990032,
0.0842175114474169));
#11431=CARTESIAN_POINT('Ctrl Pts',(-0.975530745318961,-0.224161999508995,
0.104422493053066));
#11432=CARTESIAN_POINT('Ctrl Pts',(-0.971100730005489,-0.203463743702801,
0.139836317888042));
#11433=CARTESIAN_POINT('Ctrl Pts',(-0.968453058988463,-0.190326085855194,
0.15681442133453));
#11434=CARTESIAN_POINT('Ctrl Pts',(-0.963103647174702,-0.15976606450048,
0.1868781821531));
#11435=CARTESIAN_POINT('Ctrl Pts',(-0.960411259488514,-0.142345102874864,
0.199966927975188));
#11436=CARTESIAN_POINT('Ctrl Pts',(-0.955173119738174,-0.099930567888331,
0.223801617934945));
#11437=CARTESIAN_POINT('Ctrl Pts',(-0.952850216871763,-0.0740444353928835,
0.233157223576061));
#11438=CARTESIAN_POINT('Ctrl Pts',(-0.951592097314,-0.04763,0.238183666596899));
#11439=CARTESIAN_POINT('Origin',(0.,-0.04763,0.));
#11440=CARTESIAN_POINT('',(-0.841298510752802,-0.04763,-0.504455939115715));
#11441=CARTESIAN_POINT('Origin',(0.,-0.04763,0.));
#11442=CARTESIAN_POINT('Origin',(-0.707106781186547,-0.04763,-0.707106781186548));
#11443=CARTESIAN_POINT('Origin',(-0.707106781186547,0.,-0.707106781186548));
#11444=CARTESIAN_POINT('',(-0.504455939115715,-0.04763,-0.841298510752802));
#11445=CARTESIAN_POINT('Ctrl Pts',(-0.504455939115715,-0.04763,-0.841298510752802));
#11446=CARTESIAN_POINT('Ctrl Pts',(-0.508899795931835,-0.0740444353928835,
-0.838633903678357));
#11447=CARTESIAN_POINT('Ctrl Pts',(-0.517157748491652,-0.0999305678883309,
-0.833661031856294));
#11448=CARTESIAN_POINT('Ctrl Pts',(-0.537715343527944,-0.142345102874864,
-0.820511285096538));
#11449=CARTESIAN_POINT('Ctrl Pts',(-0.548874290046456,-0.159766064500479,
-0.813159949759));
#11450=CARTESIAN_POINT('Ctrl Pts',(-0.573915184558107,-0.190326085855194,
-0.795684265985089));
#11451=CARTESIAN_POINT('Ctrl Pts',(-0.587792702767295,-0.203463743702801,
-0.78555112003688));
#11452=CARTESIAN_POINT('Ctrl Pts',(-0.615966552324775,-0.224161999508995,
-0.763642258217233));
#11453=CARTESIAN_POINT('Ctrl Pts',(-0.631684198665438,-0.232861760990032,
-0.750785745543687));
#11454=CARTESIAN_POINT('Ctrl Pts',(-0.663382628119203,-0.244251601209411,
-0.722929908501543));
#11455=CARTESIAN_POINT('Ctrl Pts',(-0.679352081686668,-0.246942143572133,
-0.707917883896095));
#11456=CARTESIAN_POINT('Ctrl Pts',(-0.707917883896095,-0.246942143572133,
-0.679352081686668));
#11457=CARTESIAN_POINT('Ctrl Pts',(-0.722929908501543,-0.244251601209411,
-0.663382628119203));
#11458=CARTESIAN_POINT('Ctrl Pts',(-0.750785745543687,-0.232861760990032,
-0.631684198665439));
#11459=CARTESIAN_POINT('Ctrl Pts',(-0.763642258217232,-0.224161999508995,
-0.615966552324775));
#11460=CARTESIAN_POINT('Ctrl Pts',(-0.78555112003688,-0.203463743702801,
-0.587792702767295));
#11461=CARTESIAN_POINT('Ctrl Pts',(-0.795684265985088,-0.190326085855194,
-0.573915184558107));
#11462=CARTESIAN_POINT('Ctrl Pts',(-0.813159949759,-0.15976606450048,-0.548874290046456));
#11463=CARTESIAN_POINT('Ctrl Pts',(-0.820511285096538,-0.142345102874864,
-0.537715343527944));
#11464=CARTESIAN_POINT('Ctrl Pts',(-0.833661031856294,-0.0999305678883311,
-0.517157748491652));
#11465=CARTESIAN_POINT('Ctrl Pts',(-0.838633903678357,-0.0740444353928836,
-0.508899795931835));
#11466=CARTESIAN_POINT('Ctrl Pts',(-0.841298510752801,-0.04763,-0.504455939115715));
#11467=CARTESIAN_POINT('Origin',(-0.707106781186547,-0.04763,-0.707106781186548));
#11468=CARTESIAN_POINT('Origin',(0.,-0.04763,0.));
#11469=CARTESIAN_POINT('',(-0.238183666596899,-0.04763,-0.951592097314));
#11470=CARTESIAN_POINT('Origin',(0.,-0.04763,0.));
#11471=CARTESIAN_POINT('Origin',(5.55111512312578E-17,-0.04763,-1.));
#11472=CARTESIAN_POINT('Origin',(5.55111512312578E-17,0.,-1.));
#11473=CARTESIAN_POINT('',(0.238183666596899,-0.04763,-0.951592097314));
#11474=CARTESIAN_POINT('Ctrl Pts',(0.238183666596899,-0.04763,-0.951592097314));
#11475=CARTESIAN_POINT('Ctrl Pts',(0.233157223576062,-0.0740444353928835,
-0.952850216871763));
#11476=CARTESIAN_POINT('Ctrl Pts',(0.223801617934946,-0.099930567888331,
-0.955173119738174));
#11477=CARTESIAN_POINT('Ctrl Pts',(0.199966927975188,-0.142345102874864,
-0.960411259488514));
#11478=CARTESIAN_POINT('Ctrl Pts',(0.1868781821531,-0.15976606450048,-0.963103647174702));
#11479=CARTESIAN_POINT('Ctrl Pts',(0.15681442133453,-0.190326085855194,
-0.968453058988463));
#11480=CARTESIAN_POINT('Ctrl Pts',(0.139836317888042,-0.203463743702801,
-0.971100730005489));
#11481=CARTESIAN_POINT('Ctrl Pts',(0.104422493053067,-0.224161999508995,
-0.975530745318961));
#11482=CARTESIAN_POINT('Ctrl Pts',(0.0842175114474173,-0.232861760990032,
-0.977553872336861));
#11483=CARTESIAN_POINT('Ctrl Pts',(0.0421062857595698,-0.244251601209411,
-0.980270995488453));
#11484=CARTESIAN_POINT('Ctrl Pts',(0.0201990724523194,-0.246942143572133,
-0.980948));
#11485=CARTESIAN_POINT('Ctrl Pts',(-0.0201990724523193,-0.246942143572133,
-0.980948));
#11486=CARTESIAN_POINT('Ctrl Pts',(-0.0421062857595697,-0.244251601209411,
-0.980270995488453));
#11487=CARTESIAN_POINT('Ctrl Pts',(-0.0842175114474171,-0.232861760990032,
-0.977553872336861));
#11488=CARTESIAN_POINT('Ctrl Pts',(-0.104422493053067,-0.224161999508995,
-0.975530745318961));
#11489=CARTESIAN_POINT('Ctrl Pts',(-0.139836317888042,-0.203463743702801,
-0.971100730005489));
#11490=CARTESIAN_POINT('Ctrl Pts',(-0.15681442133453,-0.190326085855194,
-0.968453058988463));
#11491=CARTESIAN_POINT('Ctrl Pts',(-0.1868781821531,-0.15976606450048,-0.963103647174702));
#11492=CARTESIAN_POINT('Ctrl Pts',(-0.199966927975188,-0.142345102874864,
-0.960411259488514));
#11493=CARTESIAN_POINT('Ctrl Pts',(-0.223801617934945,-0.099930567888331,
-0.955173119738174));
#11494=CARTESIAN_POINT('Ctrl Pts',(-0.233157223576062,-0.0740444353928835,
-0.952850216871763));
#11495=CARTESIAN_POINT('Ctrl Pts',(-0.238183666596899,-0.0476299999999999,
-0.951592097314));
#11496=CARTESIAN_POINT('Origin',(5.55111512312578E-17,-0.04763,-1.));
#11497=CARTESIAN_POINT('Origin',(0.,-0.04763,0.));
#11498=CARTESIAN_POINT('',(0.504455939115715,-0.04763,-0.841298510752802));
#11499=CARTESIAN_POINT('Origin',(0.,-0.04763,0.));
#11500=CARTESIAN_POINT('Origin',(0.707106781186548,-0.04763,-0.707106781186547));
#11501=CARTESIAN_POINT('Origin',(0.707106781186548,0.,-0.707106781186547));
#11502=CARTESIAN_POINT('',(0.841298510752802,-0.04763,-0.504455939115715));
#11503=CARTESIAN_POINT('Ctrl Pts',(0.841298510752802,-0.04763,-0.504455939115715));
#11504=CARTESIAN_POINT('Ctrl Pts',(0.838633903678357,-0.0740444353928835,
-0.508899795931835));
#11505=CARTESIAN_POINT('Ctrl Pts',(0.833661031856294,-0.0999305678883309,
-0.517157748491652));
#11506=CARTESIAN_POINT('Ctrl Pts',(0.820511285096538,-0.142345102874864,
-0.537715343527944));
#11507=CARTESIAN_POINT('Ctrl Pts',(0.813159949759,-0.159766064500479,-0.548874290046456));
#11508=CARTESIAN_POINT('Ctrl Pts',(0.795684265985088,-0.190326085855194,
-0.573915184558107));
#11509=CARTESIAN_POINT('Ctrl Pts',(0.78555112003688,-0.203463743702801,
-0.587792702767295));
#11510=CARTESIAN_POINT('Ctrl Pts',(0.763642258217233,-0.224161999508995,
-0.615966552324775));
#11511=CARTESIAN_POINT('Ctrl Pts',(0.750785745543687,-0.232861760990032,
-0.631684198665438));
#11512=CARTESIAN_POINT('Ctrl Pts',(0.722929908501543,-0.244251601209411,
-0.663382628119203));
#11513=CARTESIAN_POINT('Ctrl Pts',(0.707917883896095,-0.246942143572133,
-0.679352081686668));
#11514=CARTESIAN_POINT('Ctrl Pts',(0.679352081686668,-0.246942143572133,
-0.707917883896095));
#11515=CARTESIAN_POINT('Ctrl Pts',(0.663382628119203,-0.244251601209411,
-0.722929908501543));
#11516=CARTESIAN_POINT('Ctrl Pts',(0.631684198665438,-0.232861760990032,
-0.750785745543687));
#11517=CARTESIAN_POINT('Ctrl Pts',(0.615966552324775,-0.224161999508995,
-0.763642258217232));
#11518=CARTESIAN_POINT('Ctrl Pts',(0.587792702767295,-0.203463743702801,
-0.78555112003688));
#11519=CARTESIAN_POINT('Ctrl Pts',(0.573915184558107,-0.190326085855194,
-0.795684265985088));
#11520=CARTESIAN_POINT('Ctrl Pts',(0.548874290046456,-0.159766064500479,
-0.813159949759));
#11521=CARTESIAN_POINT('Ctrl Pts',(0.537715343527944,-0.142345102874864,
-0.820511285096538));
#11522=CARTESIAN_POINT('Ctrl Pts',(0.517157748491652,-0.099930567888331,
-0.833661031856294));
#11523=CARTESIAN_POINT('Ctrl Pts',(0.508899795931835,-0.0740444353928835,
-0.838633903678357));
#11524=CARTESIAN_POINT('Ctrl Pts',(0.504455939115715,-0.04763,-0.841298510752801));
#11525=CARTESIAN_POINT('Origin',(0.707106781186548,-0.04763,-0.707106781186547));
#11526=CARTESIAN_POINT('Origin',(0.,-0.166705,0.));
#11527=CARTESIAN_POINT('',(-0.980948,-0.28578,1.20131482833E-16));
#11528=CARTESIAN_POINT('Origin',(0.,-0.28578,0.));
#11529=CARTESIAN_POINT('',(-0.980948,-0.166705,1.20131482833E-16));
#11530=CARTESIAN_POINT('',(0.951592097314,-0.04763,0.238183666596899));
#11531=CARTESIAN_POINT('Origin',(0.,-0.04763,0.));
#11532=CARTESIAN_POINT('',(0.951592097314,-0.04763,-0.238183666596899));
#11533=CARTESIAN_POINT('Ctrl Pts',(0.951592097314,-0.04763,0.238183666596899));
#11534=CARTESIAN_POINT('Ctrl Pts',(0.952850216871763,-0.0740444353928835,
0.233157223576062));
#11535=CARTESIAN_POINT('Ctrl Pts',(0.955173119738174,-0.099930567888331,
0.223801617934945));
#11536=CARTESIAN_POINT('Ctrl Pts',(0.960411259488514,-0.142345102874864,
0.199966927975188));
#11537=CARTESIAN_POINT('Ctrl Pts',(0.963103647174702,-0.15976606450048,
0.1868781821531));
#11538=CARTESIAN_POINT('Ctrl Pts',(0.968453058988463,-0.190326085855194,
0.15681442133453));
#11539=CARTESIAN_POINT('Ctrl Pts',(0.971100730005489,-0.203463743702801,
0.139836317888042));
#11540=CARTESIAN_POINT('Ctrl Pts',(0.975530745318961,-0.224161999508995,
0.104422493053067));
#11541=CARTESIAN_POINT('Ctrl Pts',(0.977553872336861,-0.232861760990032,
0.0842175114474172));
#11542=CARTESIAN_POINT('Ctrl Pts',(0.980270995488453,-0.244251601209411,
0.0421062857595697));
#11543=CARTESIAN_POINT('Ctrl Pts',(0.980948,-0.246942143572133,0.0201990724523194));
#11544=CARTESIAN_POINT('Ctrl Pts',(0.980948,-0.246942143572133,-0.0201990724523194));
#11545=CARTESIAN_POINT('Ctrl Pts',(0.980270995488453,-0.244251601209411,
-0.0421062857595697));
#11546=CARTESIAN_POINT('Ctrl Pts',(0.977553872336861,-0.232861760990032,
-0.0842175114474172));
#11547=CARTESIAN_POINT('Ctrl Pts',(0.975530745318961,-0.224161999508995,
-0.104422493053067));
#11548=CARTESIAN_POINT('Ctrl Pts',(0.971100730005489,-0.203463743702801,
-0.139836317888042));
#11549=CARTESIAN_POINT('Ctrl Pts',(0.968453058988463,-0.190326085855194,
-0.15681442133453));
#11550=CARTESIAN_POINT('Ctrl Pts',(0.963103647174702,-0.15976606450048,
-0.1868781821531));
#11551=CARTESIAN_POINT('Ctrl Pts',(0.960411259488514,-0.142345102874864,
-0.199966927975188));
#11552=CARTESIAN_POINT('Ctrl Pts',(0.955173119738174,-0.099930567888331,
-0.223801617934945));
#11553=CARTESIAN_POINT('Ctrl Pts',(0.952850216871763,-0.0740444353928835,
-0.233157223576062));
#11554=CARTESIAN_POINT('Ctrl Pts',(0.951592097314,-0.0476299999999999,-0.238183666596899));
#11555=CARTESIAN_POINT('Origin',(0.,-0.04763,0.));
#11556=CARTESIAN_POINT('Origin',(0.,-0.04763,0.));
#11557=CARTESIAN_POINT('Origin',(1.,-0.04763,0.));
#11558=CARTESIAN_POINT('Origin',(1.,0.,0.));
#11559=CARTESIAN_POINT('Origin',(1.,-0.04763,0.));
#11560=CARTESIAN_POINT('Origin',(0.,-0.28578,0.));
#11561=CARTESIAN_POINT('Origin',(0.,-0.04763,0.));
#11562=CARTESIAN_POINT('',(0.,0.,0.));
#11563=CARTESIAN_POINT('Origin',(1.013815,0.445,0.));
#11564=CARTESIAN_POINT('',(-1.013815,0.445,-1.24156529467757E-16));
#11565=CARTESIAN_POINT('Origin',(0.,0.445,0.));
#11566=CARTESIAN_POINT('',(-0.991185,0.445,-1.21385153761287E-16));
#11567=CARTESIAN_POINT('Origin',(0.,0.445,0.));
#11568=CARTESIAN_POINT('Origin',(0.,0.4075,0.));
#11569=CARTESIAN_POINT('',(-1.013815,0.37,-1.24156529467757E-16));
#11570=CARTESIAN_POINT('Origin',(0.,0.37,0.));
#11571=CARTESIAN_POINT('',(-1.013815,0.4075,-1.24156529467757E-16));
#11572=CARTESIAN_POINT('Origin',(0.991185,0.37,0.));
#11573=CARTESIAN_POINT('',(-0.991185,0.37,-1.21385153761287E-16));
#11574=CARTESIAN_POINT('Origin',(0.,0.37,0.));
#11575=CARTESIAN_POINT('Origin',(0.,0.4075,0.));
#11576=CARTESIAN_POINT('',(-0.991185,0.4075,-1.21385153761287E-16));
#11577=CARTESIAN_POINT('Origin',(1.013815,-0.37,0.));
#11578=CARTESIAN_POINT('',(-1.013815,-0.37,-1.24156529467757E-16));
#11579=CARTESIAN_POINT('Origin',(0.,-0.37,0.));
#11580=CARTESIAN_POINT('',(-0.991185,-0.37,-1.21385153761287E-16));
#11581=CARTESIAN_POINT('Origin',(0.,-0.37,0.));
#11582=CARTESIAN_POINT('Origin',(0.,-0.4075,0.));
#11583=CARTESIAN_POINT('',(-1.013815,-0.445,-1.24156529467757E-16));
#11584=CARTESIAN_POINT('Origin',(0.,-0.445,0.));
#11585=CARTESIAN_POINT('',(-1.013815,-0.4075,-1.24156529467757E-16));
#11586=CARTESIAN_POINT('Origin',(0.991185,-0.445,0.));
#11587=CARTESIAN_POINT('',(-0.991185,-0.445,-1.21385153761287E-16));
#11588=CARTESIAN_POINT('Origin',(0.,-0.445,0.));
#11589=CARTESIAN_POINT('Origin',(0.,-0.4075,0.));
#11590=CARTESIAN_POINT('',(-0.991185,-0.4075,-1.21385153761287E-16));
#11591=CARTESIAN_POINT('',(0.,0.,0.));
#11592=CARTESIAN_POINT('',(0.,0.,0.));
#11593=CARTESIAN_POINT('',(0.,0.,0.));
#11594=CARTESIAN_POINT('',(0.,0.,0.));
#11595=CARTESIAN_POINT('',(0.,0.,0.));
#11596=CARTESIAN_POINT('',(0.,0.,0.));
#11597=CARTESIAN_POINT('Origin',(-2.,-10.45,5.));
#11598=CARTESIAN_POINT('',(-3.5,-9.55,5.));
#11599=CARTESIAN_POINT('Origin',(-2.,-9.55,5.));
#11600=CARTESIAN_POINT('',(-3.5,-10.45,5.));
#11601=CARTESIAN_POINT('',(-3.5,-10.45,5.));
#11602=CARTESIAN_POINT('Origin',(-2.,-10.45,5.));
#11603=CARTESIAN_POINT('Origin',(-2.,-10.45,5.));
#11604=CARTESIAN_POINT('',(-3.8,-9.55,5.));
#11605=CARTESIAN_POINT('Origin',(-2.,-9.55,5.));
#11606=CARTESIAN_POINT('',(-3.8,-10.45,5.));
#11607=CARTESIAN_POINT('',(-3.8,-10.45,5.));
#11608=CARTESIAN_POINT('Origin',(-2.,-10.45,5.));
#11609=CARTESIAN_POINT('Origin',(-2.,-9.55,5.));
#11610=CARTESIAN_POINT('Origin',(-2.,-10.45,5.));
#11611=CARTESIAN_POINT('',(0.,0.,0.));
#11612=CARTESIAN_POINT('Origin',(-2.,-10.65,5.));
#11613=CARTESIAN_POINT('',(-3.1,-10.45,5.));
#11614=CARTESIAN_POINT('Origin',(-2.,-10.45,5.));
#11615=CARTESIAN_POINT('',(-3.1,-10.65,5.));
#11616=CARTESIAN_POINT('',(-3.1,-10.65,5.));
#11617=CARTESIAN_POINT('Origin',(-2.,-10.65,5.));
#11618=CARTESIAN_POINT('Origin',(-2.,-10.65,5.));
#11619=CARTESIAN_POINT('',(-3.8,-10.45,5.));
#11620=CARTESIAN_POINT('Origin',(-2.,-10.45,5.));
#11621=CARTESIAN_POINT('',(-3.8,-10.65,5.));
#11622=CARTESIAN_POINT('',(-3.8,-10.65,5.));
#11623=CARTESIAN_POINT('Origin',(-2.,-10.65,5.));
#11624=CARTESIAN_POINT('Origin',(-2.,-10.45,5.));
#11625=CARTESIAN_POINT('Origin',(-2.,-10.65,5.));
#11626=CARTESIAN_POINT('',(0.,0.,0.));
#11627=CARTESIAN_POINT('Origin',(-2.,-9.55,5.));
#11628=CARTESIAN_POINT('',(-3.1,-9.35,5.));
#11629=CARTESIAN_POINT('Origin',(-2.,-9.35,5.));
#11630=CARTESIAN_POINT('',(-3.1,-9.55,5.));
#11631=CARTESIAN_POINT('',(-3.1,-9.55,5.));
#11632=CARTESIAN_POINT('Origin',(-2.,-9.55,5.));
#11633=CARTESIAN_POINT('Origin',(-2.,-9.55,5.));
#11634=CARTESIAN_POINT('',(-3.8,-9.35,5.));
#11635=CARTESIAN_POINT('Origin',(-2.,-9.35,5.));
#11636=CARTESIAN_POINT('',(-3.8,-9.55,5.));
#11637=CARTESIAN_POINT('',(-3.8,-9.55,5.));
#11638=CARTESIAN_POINT('Origin',(-2.,-9.55,5.));
#11639=CARTESIAN_POINT('Origin',(-2.,-9.35,5.));
#11640=CARTESIAN_POINT('Origin',(-2.,-9.55,5.));
#11641=CARTESIAN_POINT('',(-2.,-10.,5.));
#11642=CARTESIAN_POINT('',(0.,0.,0.));
#11643=CARTESIAN_POINT('',(0.,0.,0.));
#11644=CARTESIAN_POINT('',(0.,0.,0.));
#11645=CARTESIAN_POINT('',(0.,0.,0.));
#11646=CARTESIAN_POINT('',(0.,0.,0.));
#11647=CARTESIAN_POINT('',(0.,0.,0.));
#11648=CARTESIAN_POINT('',(4.,-1.77635683940025E-15,0.));
#11649=CARTESIAN_POINT('',(3.62016648949173,20.,-0.135665540738419));
#11650=CARTESIAN_POINT('',(0.255394572677749,20.,0.10988800521545));
#11651=UNCERTAINTY_MEASURE_WITH_UNIT(LENGTH_MEASURE(0.001),#11749,
'DISTANCE_ACCURACY_VALUE',
'Maximum model space distance between geometric entities at asserted c
onnectivities');
#11652=UNCERTAINTY_MEASURE_WITH_UNIT(LENGTH_MEASURE(0.001),#11749,
'DISTANCE_ACCURACY_VALUE',
'Maximum model space distance between geometric entities at asserted c
onnectivities');
#11653=UNCERTAINTY_MEASURE_WITH_UNIT(LENGTH_MEASURE(0.001),#11749,
'DISTANCE_ACCURACY_VALUE',
'Maximum model space distance between geometric entities at asserted c
onnectivities');
#11654=UNCERTAINTY_MEASURE_WITH_UNIT(LENGTH_MEASURE(0.001),#11749,
'DISTANCE_ACCURACY_VALUE',
'Maximum model space distance between geometric entities at asserted c
onnectivities');
#11655=UNCERTAINTY_MEASURE_WITH_UNIT(LENGTH_MEASURE(0.001),#11749,
'DISTANCE_ACCURACY_VALUE',
'Maximum model space distance between geometric entities at asserted c
onnectivities');
#11656=UNCERTAINTY_MEASURE_WITH_UNIT(LENGTH_MEASURE(0.001),#11749,
'DISTANCE_ACCURACY_VALUE',
'Maximum model space distance between geometric entities at asserted c
onnectivities');
#11657=UNCERTAINTY_MEASURE_WITH_UNIT(LENGTH_MEASURE(0.001),#11749,
'DISTANCE_ACCURACY_VALUE',
'Maximum model space distance between geometric entities at asserted c
onnectivities');
#11658=UNCERTAINTY_MEASURE_WITH_UNIT(LENGTH_MEASURE(0.001),#11749,
'DISTANCE_ACCURACY_VALUE',
'Maximum model space distance between geometric entities at asserted c
onnectivities');
#11659=UNCERTAINTY_MEASURE_WITH_UNIT(LENGTH_MEASURE(0.001),#11749,
'DISTANCE_ACCURACY_VALUE',
'Maximum model space distance between geometric entities at asserted c
onnectivities');
#11660=UNCERTAINTY_MEASURE_WITH_UNIT(LENGTH_MEASURE(0.001),#11749,
'DISTANCE_ACCURACY_VALUE',
'Maximum model space distance between geometric entities at asserted c
onnectivities');
#11661=UNCERTAINTY_MEASURE_WITH_UNIT(LENGTH_MEASURE(0.001),#11749,
'DISTANCE_ACCURACY_VALUE',
'Maximum model space distance between geometric entities at asserted c
onnectivities');
#11662=UNCERTAINTY_MEASURE_WITH_UNIT(LENGTH_MEASURE(0.001),#11749,
'DISTANCE_ACCURACY_VALUE',
'Maximum model space distance between geometric entities at asserted c
onnectivities');
#11663=UNCERTAINTY_MEASURE_WITH_UNIT(LENGTH_MEASURE(0.001),#11749,
'DISTANCE_ACCURACY_VALUE',
'Maximum model space distance between geometric entities at asserted c
onnectivities');
#11664=UNCERTAINTY_MEASURE_WITH_UNIT(LENGTH_MEASURE(0.001),#11749,
'DISTANCE_ACCURACY_VALUE',
'Maximum model space distance between geometric entities at asserted c
onnectivities');
#11665=UNCERTAINTY_MEASURE_WITH_UNIT(LENGTH_MEASURE(0.001),#11749,
'DISTANCE_ACCURACY_VALUE',
'Maximum model space distance between geometric entities at asserted c
onnectivities');
#11666=UNCERTAINTY_MEASURE_WITH_UNIT(LENGTH_MEASURE(0.001),#11749,
'DISTANCE_ACCURACY_VALUE',
'Maximum model space distance between geometric entities at asserted c
onnectivities');
#11667=UNCERTAINTY_MEASURE_WITH_UNIT(LENGTH_MEASURE(0.001),#11749,
'DISTANCE_ACCURACY_VALUE',
'Maximum model space distance between geometric entities at asserted c
onnectivities');
#11668=UNCERTAINTY_MEASURE_WITH_UNIT(LENGTH_MEASURE(0.001),#11749,
'DISTANCE_ACCURACY_VALUE',
'Maximum model space distance between geometric entities at asserted c
onnectivities');
#11669=UNCERTAINTY_MEASURE_WITH_UNIT(LENGTH_MEASURE(0.001),#11749,
'DISTANCE_ACCURACY_VALUE',
'Maximum model space distance between geometric entities at asserted c
onnectivities');
#11670=UNCERTAINTY_MEASURE_WITH_UNIT(LENGTH_MEASURE(0.001),#11749,
'DISTANCE_ACCURACY_VALUE',
'Maximum model space distance between geometric entities at asserted c
onnectivities');
#11671=UNCERTAINTY_MEASURE_WITH_UNIT(LENGTH_MEASURE(0.001),#11749,
'DISTANCE_ACCURACY_VALUE',
'Maximum model space distance between geometric entities at asserted c
onnectivities');
#11672=UNCERTAINTY_MEASURE_WITH_UNIT(LENGTH_MEASURE(0.001),#11749,
'DISTANCE_ACCURACY_VALUE',
'Maximum model space distance between geometric entities at asserted c
onnectivities');
#11673=UNCERTAINTY_MEASURE_WITH_UNIT(LENGTH_MEASURE(0.001),#11749,
'DISTANCE_ACCURACY_VALUE',
'Maximum model space distance between geometric entities at asserted c
onnectivities');
#11674=UNCERTAINTY_MEASURE_WITH_UNIT(LENGTH_MEASURE(0.001),#11749,
'DISTANCE_ACCURACY_VALUE',
'Maximum model space distance between geometric entities at asserted c
onnectivities');
#11675=UNCERTAINTY_MEASURE_WITH_UNIT(LENGTH_MEASURE(0.001),#11749,
'DISTANCE_ACCURACY_VALUE',
'Maximum model space distance between geometric entities at asserted c
onnectivities');
#11676=UNCERTAINTY_MEASURE_WITH_UNIT(LENGTH_MEASURE(0.001),#11749,
'DISTANCE_ACCURACY_VALUE',
'Maximum model space distance between geometric entities at asserted c
onnectivities');
#11677=UNCERTAINTY_MEASURE_WITH_UNIT(LENGTH_MEASURE(0.001),#11749,
'DISTANCE_ACCURACY_VALUE',
'Maximum model space distance between geometric entities at asserted c
onnectivities');
#11678=UNCERTAINTY_MEASURE_WITH_UNIT(LENGTH_MEASURE(0.001),#11749,
'DISTANCE_ACCURACY_VALUE',
'Maximum model space distance between geometric entities at asserted c
onnectivities');
#11679=UNCERTAINTY_MEASURE_WITH_UNIT(LENGTH_MEASURE(0.001),#11749,
'DISTANCE_ACCURACY_VALUE',
'Maximum model space distance between geometric entities at asserted c
onnectivities');
#11680=UNCERTAINTY_MEASURE_WITH_UNIT(LENGTH_MEASURE(0.001),#11749,
'DISTANCE_ACCURACY_VALUE',
'Maximum model space distance between geometric entities at asserted c
onnectivities');
#11681=UNCERTAINTY_MEASURE_WITH_UNIT(LENGTH_MEASURE(0.001),#11749,
'DISTANCE_ACCURACY_VALUE',
'Maximum model space distance between geometric entities at asserted c
onnectivities');
#11682=UNCERTAINTY_MEASURE_WITH_UNIT(LENGTH_MEASURE(0.001),#11749,
'DISTANCE_ACCURACY_VALUE',
'Maximum model space distance between geometric entities at asserted c
onnectivities');
#11683=UNCERTAINTY_MEASURE_WITH_UNIT(LENGTH_MEASURE(0.001),#11749,
'DISTANCE_ACCURACY_VALUE',
'Maximum model space distance between geometric entities at asserted c
onnectivities');
#11684=UNCERTAINTY_MEASURE_WITH_UNIT(LENGTH_MEASURE(0.001),#11749,
'DISTANCE_ACCURACY_VALUE',
'Maximum model space distance between geometric entities at asserted c
onnectivities');
#11685=UNCERTAINTY_MEASURE_WITH_UNIT(LENGTH_MEASURE(0.001),#11749,
'DISTANCE_ACCURACY_VALUE',
'Maximum model space distance between geometric entities at asserted c
onnectivities');
#11686=UNCERTAINTY_MEASURE_WITH_UNIT(LENGTH_MEASURE(0.001),#11749,
'DISTANCE_ACCURACY_VALUE',
'Maximum model space distance between geometric entities at asserted c
onnectivities');
#11687=UNCERTAINTY_MEASURE_WITH_UNIT(LENGTH_MEASURE(0.001),#11749,
'DISTANCE_ACCURACY_VALUE',
'Maximum model space distance between geometric entities at asserted c
onnectivities');
#11688=UNCERTAINTY_MEASURE_WITH_UNIT(LENGTH_MEASURE(0.001),#11749,
'DISTANCE_ACCURACY_VALUE',
'Maximum model space distance between geometric entities at asserted c
onnectivities');
#11689=UNCERTAINTY_MEASURE_WITH_UNIT(LENGTH_MEASURE(0.001),#11749,
'DISTANCE_ACCURACY_VALUE',
'Maximum model space distance between geometric entities at asserted c
onnectivities');
#11690=UNCERTAINTY_MEASURE_WITH_UNIT(LENGTH_MEASURE(0.001),#11749,
'DISTANCE_ACCURACY_VALUE',
'Maximum model space distance between geometric entities at asserted c
onnectivities');
#11691=UNCERTAINTY_MEASURE_WITH_UNIT(LENGTH_MEASURE(0.001),#11749,
'DISTANCE_ACCURACY_VALUE',
'Maximum model space distance between geometric entities at asserted c
onnectivities');
#11692=UNCERTAINTY_MEASURE_WITH_UNIT(LENGTH_MEASURE(0.001),#11749,
'DISTANCE_ACCURACY_VALUE',
'Maximum model space distance between geometric entities at asserted c
onnectivities');
#11693=UNCERTAINTY_MEASURE_WITH_UNIT(LENGTH_MEASURE(0.001),#11749,
'DISTANCE_ACCURACY_VALUE',
'Maximum model space distance between geometric entities at asserted c
onnectivities');
#11694=UNCERTAINTY_MEASURE_WITH_UNIT(LENGTH_MEASURE(0.001),#11749,
'DISTANCE_ACCURACY_VALUE',
'Maximum model space distance between geometric entities at asserted c
onnectivities');
#11695=UNCERTAINTY_MEASURE_WITH_UNIT(LENGTH_MEASURE(0.001),#11749,
'DISTANCE_ACCURACY_VALUE',
'Maximum model space distance between geometric entities at asserted c
onnectivities');
#11696=UNCERTAINTY_MEASURE_WITH_UNIT(LENGTH_MEASURE(0.001),#11749,
'DISTANCE_ACCURACY_VALUE',
'Maximum model space distance between geometric entities at asserted c
onnectivities');
#11697=UNCERTAINTY_MEASURE_WITH_UNIT(LENGTH_MEASURE(0.001),#11749,
'DISTANCE_ACCURACY_VALUE',
'Maximum model space distance between geometric entities at asserted c
onnectivities');
#11698=UNCERTAINTY_MEASURE_WITH_UNIT(LENGTH_MEASURE(0.001),#11749,
'DISTANCE_ACCURACY_VALUE',
'Maximum model space distance between geometric entities at asserted c
onnectivities');
#11699=UNCERTAINTY_MEASURE_WITH_UNIT(LENGTH_MEASURE(0.001),#11749,
'DISTANCE_ACCURACY_VALUE',
'Maximum model space distance between geometric entities at asserted c
onnectivities');
#11700=(
GEOMETRIC_REPRESENTATION_CONTEXT(3)
GLOBAL_UNCERTAINTY_ASSIGNED_CONTEXT((#11651))
GLOBAL_UNIT_ASSIGNED_CONTEXT((#11749,#11751,#11752))
REPRESENTATION_CONTEXT('','3D')
);
#11701=(
GEOMETRIC_REPRESENTATION_CONTEXT(3)
GLOBAL_UNCERTAINTY_ASSIGNED_CONTEXT((#11652))
GLOBAL_UNIT_ASSIGNED_CONTEXT((#11749,#11751,#11752))
REPRESENTATION_CONTEXT('','3D')
);
#11702=(
GEOMETRIC_REPRESENTATION_CONTEXT(3)
GLOBAL_UNCERTAINTY_ASSIGNED_CONTEXT((#11653))
GLOBAL_UNIT_ASSIGNED_CONTEXT((#11749,#11751,#11752))
REPRESENTATION_CONTEXT('','3D')
);
#11703=(
GEOMETRIC_REPRESENTATION_CONTEXT(3)
GLOBAL_UNCERTAINTY_ASSIGNED_CONTEXT((#11654))
GLOBAL_UNIT_ASSIGNED_CONTEXT((#11749,#11751,#11752))
REPRESENTATION_CONTEXT('','3D')
);
#11704=(
GEOMETRIC_REPRESENTATION_CONTEXT(3)
GLOBAL_UNCERTAINTY_ASSIGNED_CONTEXT((#11655))
GLOBAL_UNIT_ASSIGNED_CONTEXT((#11749,#11751,#11752))
REPRESENTATION_CONTEXT('','3D')
);
#11705=(
GEOMETRIC_REPRESENTATION_CONTEXT(3)
GLOBAL_UNCERTAINTY_ASSIGNED_CONTEXT((#11656))
GLOBAL_UNIT_ASSIGNED_CONTEXT((#11749,#11751,#11752))
REPRESENTATION_CONTEXT('','3D')
);
#11706=(
GEOMETRIC_REPRESENTATION_CONTEXT(3)
GLOBAL_UNCERTAINTY_ASSIGNED_CONTEXT((#11657))
GLOBAL_UNIT_ASSIGNED_CONTEXT((#11749,#11751,#11752))
REPRESENTATION_CONTEXT('','3D')
);
#11707=(
GEOMETRIC_REPRESENTATION_CONTEXT(3)
GLOBAL_UNCERTAINTY_ASSIGNED_CONTEXT((#11658))
GLOBAL_UNIT_ASSIGNED_CONTEXT((#11749,#11751,#11752))
REPRESENTATION_CONTEXT('','3D')
);
#11708=(
GEOMETRIC_REPRESENTATION_CONTEXT(3)
GLOBAL_UNCERTAINTY_ASSIGNED_CONTEXT((#11659))
GLOBAL_UNIT_ASSIGNED_CONTEXT((#11749,#11751,#11752))
REPRESENTATION_CONTEXT('','3D')
);
#11709=(
GEOMETRIC_REPRESENTATION_CONTEXT(3)
GLOBAL_UNCERTAINTY_ASSIGNED_CONTEXT((#11660))
GLOBAL_UNIT_ASSIGNED_CONTEXT((#11749,#11751,#11752))
REPRESENTATION_CONTEXT('','3D')
);
#11710=(
GEOMETRIC_REPRESENTATION_CONTEXT(3)
GLOBAL_UNCERTAINTY_ASSIGNED_CONTEXT((#11661))
GLOBAL_UNIT_ASSIGNED_CONTEXT((#11749,#11751,#11752))
REPRESENTATION_CONTEXT('','3D')
);
#11711=(
GEOMETRIC_REPRESENTATION_CONTEXT(3)
GLOBAL_UNCERTAINTY_ASSIGNED_CONTEXT((#11662))
GLOBAL_UNIT_ASSIGNED_CONTEXT((#11749,#11751,#11752))
REPRESENTATION_CONTEXT('','3D')
);
#11712=(
GEOMETRIC_REPRESENTATION_CONTEXT(3)
GLOBAL_UNCERTAINTY_ASSIGNED_CONTEXT((#11663))
GLOBAL_UNIT_ASSIGNED_CONTEXT((#11749,#11751,#11752))
REPRESENTATION_CONTEXT('','3D')
);
#11713=(
GEOMETRIC_REPRESENTATION_CONTEXT(3)
GLOBAL_UNCERTAINTY_ASSIGNED_CONTEXT((#11664))
GLOBAL_UNIT_ASSIGNED_CONTEXT((#11749,#11751,#11752))
REPRESENTATION_CONTEXT('','3D')
);
#11714=(
GEOMETRIC_REPRESENTATION_CONTEXT(3)
GLOBAL_UNCERTAINTY_ASSIGNED_CONTEXT((#11665))
GLOBAL_UNIT_ASSIGNED_CONTEXT((#11749,#11751,#11752))
REPRESENTATION_CONTEXT('','3D')
);
#11715=(
GEOMETRIC_REPRESENTATION_CONTEXT(3)
GLOBAL_UNCERTAINTY_ASSIGNED_CONTEXT((#11666))
GLOBAL_UNIT_ASSIGNED_CONTEXT((#11749,#11751,#11752))
REPRESENTATION_CONTEXT('','3D')
);
#11716=(
GEOMETRIC_REPRESENTATION_CONTEXT(3)
GLOBAL_UNCERTAINTY_ASSIGNED_CONTEXT((#11667))
GLOBAL_UNIT_ASSIGNED_CONTEXT((#11749,#11751,#11752))
REPRESENTATION_CONTEXT('','3D')
);
#11717=(
GEOMETRIC_REPRESENTATION_CONTEXT(3)
GLOBAL_UNCERTAINTY_ASSIGNED_CONTEXT((#11668))
GLOBAL_UNIT_ASSIGNED_CONTEXT((#11749,#11751,#11752))
REPRESENTATION_CONTEXT('','3D')
);
#11718=(
GEOMETRIC_REPRESENTATION_CONTEXT(3)
GLOBAL_UNCERTAINTY_ASSIGNED_CONTEXT((#11669))
GLOBAL_UNIT_ASSIGNED_CONTEXT((#11749,#11751,#11752))
REPRESENTATION_CONTEXT('','3D')
);
#11719=(
GEOMETRIC_REPRESENTATION_CONTEXT(3)
GLOBAL_UNCERTAINTY_ASSIGNED_CONTEXT((#11670))
GLOBAL_UNIT_ASSIGNED_CONTEXT((#11749,#11751,#11752))
REPRESENTATION_CONTEXT('','3D')
);
#11720=(
GEOMETRIC_REPRESENTATION_CONTEXT(3)
GLOBAL_UNCERTAINTY_ASSIGNED_CONTEXT((#11671))
GLOBAL_UNIT_ASSIGNED_CONTEXT((#11749,#11751,#11752))
REPRESENTATION_CONTEXT('','3D')
);
#11721=(
GEOMETRIC_REPRESENTATION_CONTEXT(3)
GLOBAL_UNCERTAINTY_ASSIGNED_CONTEXT((#11672))
GLOBAL_UNIT_ASSIGNED_CONTEXT((#11749,#11751,#11752))
REPRESENTATION_CONTEXT('','3D')
);
#11722=(
GEOMETRIC_REPRESENTATION_CONTEXT(3)
GLOBAL_UNCERTAINTY_ASSIGNED_CONTEXT((#11673))
GLOBAL_UNIT_ASSIGNED_CONTEXT((#11749,#11751,#11752))
REPRESENTATION_CONTEXT('','3D')
);
#11723=(
GEOMETRIC_REPRESENTATION_CONTEXT(3)
GLOBAL_UNCERTAINTY_ASSIGNED_CONTEXT((#11674))
GLOBAL_UNIT_ASSIGNED_CONTEXT((#11749,#11751,#11752))
REPRESENTATION_CONTEXT('','3D')
);
#11724=(
GEOMETRIC_REPRESENTATION_CONTEXT(3)
GLOBAL_UNCERTAINTY_ASSIGNED_CONTEXT((#11675))
GLOBAL_UNIT_ASSIGNED_CONTEXT((#11749,#11751,#11752))
REPRESENTATION_CONTEXT('','3D')
);
#11725=(
GEOMETRIC_REPRESENTATION_CONTEXT(3)
GLOBAL_UNCERTAINTY_ASSIGNED_CONTEXT((#11676))
GLOBAL_UNIT_ASSIGNED_CONTEXT((#11749,#11751,#11752))
REPRESENTATION_CONTEXT('','3D')
);
#11726=(
GEOMETRIC_REPRESENTATION_CONTEXT(3)
GLOBAL_UNCERTAINTY_ASSIGNED_CONTEXT((#11677))
GLOBAL_UNIT_ASSIGNED_CONTEXT((#11749,#11751,#11752))
REPRESENTATION_CONTEXT('','3D')
);
#11727=(
GEOMETRIC_REPRESENTATION_CONTEXT(3)
GLOBAL_UNCERTAINTY_ASSIGNED_CONTEXT((#11678))
GLOBAL_UNIT_ASSIGNED_CONTEXT((#11749,#11751,#11752))
REPRESENTATION_CONTEXT('','3D')
);
#11728=(
GEOMETRIC_REPRESENTATION_CONTEXT(3)
GLOBAL_UNCERTAINTY_ASSIGNED_CONTEXT((#11679))
GLOBAL_UNIT_ASSIGNED_CONTEXT((#11749,#11751,#11752))
REPRESENTATION_CONTEXT('','3D')
);
#11729=(
GEOMETRIC_REPRESENTATION_CONTEXT(3)
GLOBAL_UNCERTAINTY_ASSIGNED_CONTEXT((#11680))
GLOBAL_UNIT_ASSIGNED_CONTEXT((#11749,#11751,#11752))
REPRESENTATION_CONTEXT('','3D')
);
#11730=(
GEOMETRIC_REPRESENTATION_CONTEXT(3)
GLOBAL_UNCERTAINTY_ASSIGNED_CONTEXT((#11681))
GLOBAL_UNIT_ASSIGNED_CONTEXT((#11749,#11751,#11752))
REPRESENTATION_CONTEXT('','3D')
);
#11731=(
GEOMETRIC_REPRESENTATION_CONTEXT(3)
GLOBAL_UNCERTAINTY_ASSIGNED_CONTEXT((#11682))
GLOBAL_UNIT_ASSIGNED_CONTEXT((#11749,#11751,#11752))
REPRESENTATION_CONTEXT('','3D')
);
#11732=(
GEOMETRIC_REPRESENTATION_CONTEXT(3)
GLOBAL_UNCERTAINTY_ASSIGNED_CONTEXT((#11683))
GLOBAL_UNIT_ASSIGNED_CONTEXT((#11749,#11751,#11752))
REPRESENTATION_CONTEXT('','3D')
);
#11733=(
GEOMETRIC_REPRESENTATION_CONTEXT(3)
GLOBAL_UNCERTAINTY_ASSIGNED_CONTEXT((#11684))
GLOBAL_UNIT_ASSIGNED_CONTEXT((#11749,#11751,#11752))
REPRESENTATION_CONTEXT('','3D')
);
#11734=(
GEOMETRIC_REPRESENTATION_CONTEXT(3)
GLOBAL_UNCERTAINTY_ASSIGNED_CONTEXT((#11685))
GLOBAL_UNIT_ASSIGNED_CONTEXT((#11749,#11751,#11752))
REPRESENTATION_CONTEXT('','3D')
);
#11735=(
GEOMETRIC_REPRESENTATION_CONTEXT(3)
GLOBAL_UNCERTAINTY_ASSIGNED_CONTEXT((#11686))
GLOBAL_UNIT_ASSIGNED_CONTEXT((#11749,#11751,#11752))
REPRESENTATION_CONTEXT('','3D')
);
#11736=(
GEOMETRIC_REPRESENTATION_CONTEXT(3)
GLOBAL_UNCERTAINTY_ASSIGNED_CONTEXT((#11687))
GLOBAL_UNIT_ASSIGNED_CONTEXT((#11749,#11751,#11752))
REPRESENTATION_CONTEXT('','3D')
);
#11737=(
GEOMETRIC_REPRESENTATION_CONTEXT(3)
GLOBAL_UNCERTAINTY_ASSIGNED_CONTEXT((#11688))
GLOBAL_UNIT_ASSIGNED_CONTEXT((#11749,#11751,#11752))
REPRESENTATION_CONTEXT('','3D')
);
#11738=(
GEOMETRIC_REPRESENTATION_CONTEXT(3)
GLOBAL_UNCERTAINTY_ASSIGNED_CONTEXT((#11689))
GLOBAL_UNIT_ASSIGNED_CONTEXT((#11749,#11751,#11752))
REPRESENTATION_CONTEXT('','3D')
);
#11739=(
GEOMETRIC_REPRESENTATION_CONTEXT(3)
GLOBAL_UNCERTAINTY_ASSIGNED_CONTEXT((#11690))
GLOBAL_UNIT_ASSIGNED_CONTEXT((#11749,#11751,#11752))
REPRESENTATION_CONTEXT('','3D')
);
#11740=(
GEOMETRIC_REPRESENTATION_CONTEXT(3)
GLOBAL_UNCERTAINTY_ASSIGNED_CONTEXT((#11691))
GLOBAL_UNIT_ASSIGNED_CONTEXT((#11749,#11751,#11752))
REPRESENTATION_CONTEXT('','3D')
);
#11741=(
GEOMETRIC_REPRESENTATION_CONTEXT(3)
GLOBAL_UNCERTAINTY_ASSIGNED_CONTEXT((#11692))
GLOBAL_UNIT_ASSIGNED_CONTEXT((#11749,#11751,#11752))
REPRESENTATION_CONTEXT('','3D')
);
#11742=(
GEOMETRIC_REPRESENTATION_CONTEXT(3)
GLOBAL_UNCERTAINTY_ASSIGNED_CONTEXT((#11693))
GLOBAL_UNIT_ASSIGNED_CONTEXT((#11749,#11751,#11752))
REPRESENTATION_CONTEXT('','3D')
);
#11743=(
GEOMETRIC_REPRESENTATION_CONTEXT(3)
GLOBAL_UNCERTAINTY_ASSIGNED_CONTEXT((#11694))
GLOBAL_UNIT_ASSIGNED_CONTEXT((#11749,#11751,#11752))
REPRESENTATION_CONTEXT('','3D')
);
#11744=(
GEOMETRIC_REPRESENTATION_CONTEXT(3)
GLOBAL_UNCERTAINTY_ASSIGNED_CONTEXT((#11695))
GLOBAL_UNIT_ASSIGNED_CONTEXT((#11749,#11751,#11752))
REPRESENTATION_CONTEXT('','3D')
);
#11745=(
GEOMETRIC_REPRESENTATION_CONTEXT(3)
GLOBAL_UNCERTAINTY_ASSIGNED_CONTEXT((#11696))
GLOBAL_UNIT_ASSIGNED_CONTEXT((#11749,#11751,#11752))
REPRESENTATION_CONTEXT('','3D')
);
#11746=(
GEOMETRIC_REPRESENTATION_CONTEXT(3)
GLOBAL_UNCERTAINTY_ASSIGNED_CONTEXT((#11697))
GLOBAL_UNIT_ASSIGNED_CONTEXT((#11749,#11751,#11752))
REPRESENTATION_CONTEXT('','3D')
);
#11747=(
GEOMETRIC_REPRESENTATION_CONTEXT(3)
GLOBAL_UNCERTAINTY_ASSIGNED_CONTEXT((#11698))
GLOBAL_UNIT_ASSIGNED_CONTEXT((#11749,#11751,#11752))
REPRESENTATION_CONTEXT('','3D')
);
#11748=(
GEOMETRIC_REPRESENTATION_CONTEXT(3)
GLOBAL_UNCERTAINTY_ASSIGNED_CONTEXT((#11699))
GLOBAL_UNIT_ASSIGNED_CONTEXT((#11749,#11751,#11752))
REPRESENTATION_CONTEXT('','3D')
);
#11749=(
LENGTH_UNIT()
NAMED_UNIT(*)
SI_UNIT(.CENTI.,.METRE.)
);
#11750=(
LENGTH_UNIT()
NAMED_UNIT(*)
SI_UNIT($,.METRE.)
);
#11751=(
NAMED_UNIT(*)
PLANE_ANGLE_UNIT()
SI_UNIT($,.RADIAN.)
);
#11752=(
NAMED_UNIT(*)
SI_UNIT($,.STERADIAN.)
SOLID_ANGLE_UNIT()
);
#11753=SHAPE_DEFINITION_REPRESENTATION(#11801,#11924);
#11754=SHAPE_DEFINITION_REPRESENTATION(#11802,#11925);
#11755=SHAPE_DEFINITION_REPRESENTATION(#11803,#11926);
#11756=SHAPE_DEFINITION_REPRESENTATION(#11804,#11927);
#11757=SHAPE_DEFINITION_REPRESENTATION(#11805,#11928);
#11758=SHAPE_DEFINITION_REPRESENTATION(#11806,#11929);
#11759=SHAPE_DEFINITION_REPRESENTATION(#11807,#11930);
#11760=SHAPE_DEFINITION_REPRESENTATION(#11808,#11931);
#11761=SHAPE_DEFINITION_REPRESENTATION(#11809,#11932);
#11762=SHAPE_DEFINITION_REPRESENTATION(#11810,#11933);
#11763=SHAPE_DEFINITION_REPRESENTATION(#11811,#11934);
#11764=SHAPE_DEFINITION_REPRESENTATION(#11812,#11935);
#11765=SHAPE_DEFINITION_REPRESENTATION(#11813,#11936);
#11766=SHAPE_DEFINITION_REPRESENTATION(#11814,#11937);
#11767=SHAPE_DEFINITION_REPRESENTATION(#11815,#11938);
#11768=SHAPE_DEFINITION_REPRESENTATION(#11816,#11939);
#11769=SHAPE_DEFINITION_REPRESENTATION(#11817,#11940);
#11770=SHAPE_DEFINITION_REPRESENTATION(#11818,#11941);
#11771=SHAPE_DEFINITION_REPRESENTATION(#11819,#11942);
#11772=SHAPE_DEFINITION_REPRESENTATION(#11820,#11943);
#11773=SHAPE_DEFINITION_REPRESENTATION(#11821,#11944);
#11774=SHAPE_DEFINITION_REPRESENTATION(#11822,#11945);
#11775=SHAPE_DEFINITION_REPRESENTATION(#11823,#11946);
#11776=SHAPE_DEFINITION_REPRESENTATION(#11824,#11947);
#11777=SHAPE_DEFINITION_REPRESENTATION(#11825,#11948);
#11778=SHAPE_DEFINITION_REPRESENTATION(#11826,#11949);
#11779=SHAPE_DEFINITION_REPRESENTATION(#11827,#11950);
#11780=SHAPE_DEFINITION_REPRESENTATION(#11828,#11951);
#11781=SHAPE_DEFINITION_REPRESENTATION(#11829,#11952);
#11782=SHAPE_DEFINITION_REPRESENTATION(#11830,#11953);
#11783=SHAPE_DEFINITION_REPRESENTATION(#11831,#11954);
#11784=SHAPE_DEFINITION_REPRESENTATION(#11832,#11955);
#11785=SHAPE_DEFINITION_REPRESENTATION(#11833,#11956);
#11786=SHAPE_DEFINITION_REPRESENTATION(#11834,#11957);
#11787=SHAPE_DEFINITION_REPRESENTATION(#11835,#11958);
#11788=SHAPE_DEFINITION_REPRESENTATION(#11836,#11959);
#11789=SHAPE_DEFINITION_REPRESENTATION(#11896,#11960);
#11790=SHAPE_DEFINITION_REPRESENTATION(#11897,#11961);
#11791=SHAPE_DEFINITION_REPRESENTATION(#11899,#11962);
#11792=SHAPE_DEFINITION_REPRESENTATION(#11900,#11963);
#11793=SHAPE_DEFINITION_REPRESENTATION(#11901,#11964);
#11794=SHAPE_DEFINITION_REPRESENTATION(#11902,#11965);
#11795=SHAPE_DEFINITION_REPRESENTATION(#11903,#11966);
#11796=SHAPE_DEFINITION_REPRESENTATION(#11904,#11967);
#11797=SHAPE_DEFINITION_REPRESENTATION(#11905,#11968);
#11798=SHAPE_DEFINITION_REPRESENTATION(#11911,#11969);
#11799=SHAPE_DEFINITION_REPRESENTATION(#11912,#11970);
#11800=SHAPE_DEFINITION_REPRESENTATION(#11913,#11971);
#11801=PRODUCT_DEFINITION_SHAPE('',$,#11973);
#11802=PRODUCT_DEFINITION_SHAPE('',$,#11974);
#11803=PRODUCT_DEFINITION_SHAPE('',$,#11975);
#11804=PRODUCT_DEFINITION_SHAPE('',$,#11976);
#11805=PRODUCT_DEFINITION_SHAPE('',$,#11977);
#11806=PRODUCT_DEFINITION_SHAPE('',$,#11978);
#11807=PRODUCT_DEFINITION_SHAPE('',$,#11979);
#11808=PRODUCT_DEFINITION_SHAPE('',$,#11980);
#11809=PRODUCT_DEFINITION_SHAPE('',$,#11981);
#11810=PRODUCT_DEFINITION_SHAPE('',$,#11982);
#11811=PRODUCT_DEFINITION_SHAPE('',$,#11983);
#11812=PRODUCT_DEFINITION_SHAPE('',$,#11984);
#11813=PRODUCT_DEFINITION_SHAPE('',$,#11985);
#11814=PRODUCT_DEFINITION_SHAPE('',$,#11986);
#11815=PRODUCT_DEFINITION_SHAPE('',$,#11987);
#11816=PRODUCT_DEFINITION_SHAPE('',$,#11988);
#11817=PRODUCT_DEFINITION_SHAPE('',$,#11989);
#11818=PRODUCT_DEFINITION_SHAPE('',$,#11990);
#11819=PRODUCT_DEFINITION_SHAPE('',$,#11991);
#11820=PRODUCT_DEFINITION_SHAPE('',$,#11992);
#11821=PRODUCT_DEFINITION_SHAPE('',$,#11993);
#11822=PRODUCT_DEFINITION_SHAPE('',$,#11994);
#11823=PRODUCT_DEFINITION_SHAPE('',$,#11995);
#11824=PRODUCT_DEFINITION_SHAPE('',$,#11996);
#11825=PRODUCT_DEFINITION_SHAPE('',$,#11997);
#11826=PRODUCT_DEFINITION_SHAPE('',$,#11998);
#11827=PRODUCT_DEFINITION_SHAPE('',$,#11999);
#11828=PRODUCT_DEFINITION_SHAPE('',$,#12000);
#11829=PRODUCT_DEFINITION_SHAPE('',$,#12001);
#11830=PRODUCT_DEFINITION_SHAPE('',$,#12002);
#11831=PRODUCT_DEFINITION_SHAPE('',$,#12003);
#11832=PRODUCT_DEFINITION_SHAPE('',$,#12004);
#11833=PRODUCT_DEFINITION_SHAPE('',$,#12005);
#11834=PRODUCT_DEFINITION_SHAPE('',$,#12006);
#11835=PRODUCT_DEFINITION_SHAPE('',$,#12007);
#11836=PRODUCT_DEFINITION_SHAPE('',$,#12008);
#11837=PRODUCT_DEFINITION_SHAPE($,$,#254);
#11838=PRODUCT_DEFINITION_SHAPE($,$,#255);
#11839=PRODUCT_DEFINITION_SHAPE($,$,#256);
#11840=PRODUCT_DEFINITION_SHAPE($,$,#257);
#11841=PRODUCT_DEFINITION_SHAPE($,$,#258);
#11842=PRODUCT_DEFINITION_SHAPE($,$,#259);
#11843=PRODUCT_DEFINITION_SHAPE($,$,#260);
#11844=PRODUCT_DEFINITION_SHAPE($,$,#261);
#11845=PRODUCT_DEFINITION_SHAPE($,$,#262);
#11846=PRODUCT_DEFINITION_SHAPE($,$,#263);
#11847=PRODUCT_DEFINITION_SHAPE($,$,#264);
#11848=PRODUCT_DEFINITION_SHAPE($,$,#265);
#11849=PRODUCT_DEFINITION_SHAPE($,$,#266);
#11850=PRODUCT_DEFINITION_SHAPE($,$,#267);
#11851=PRODUCT_DEFINITION_SHAPE($,$,#268);
#11852=PRODUCT_DEFINITION_SHAPE($,$,#269);
#11853=PRODUCT_DEFINITION_SHAPE($,$,#270);
#11854=PRODUCT_DEFINITION_SHAPE($,$,#271);
#11855=PRODUCT_DEFINITION_SHAPE($,$,#272);
#11856=PRODUCT_DEFINITION_SHAPE($,$,#273);
#11857=PRODUCT_DEFINITION_SHAPE($,$,#274);
#11858=PRODUCT_DEFINITION_SHAPE($,$,#275);
#11859=PRODUCT_DEFINITION_SHAPE($,$,#276);
#11860=PRODUCT_DEFINITION_SHAPE($,$,#277);
#11861=PRODUCT_DEFINITION_SHAPE($,$,#278);
#11862=PRODUCT_DEFINITION_SHAPE($,$,#279);
#11863=PRODUCT_DEFINITION_SHAPE($,$,#280);
#11864=PRODUCT_DEFINITION_SHAPE($,$,#281);
#11865=PRODUCT_DEFINITION_SHAPE($,$,#282);
#11866=PRODUCT_DEFINITION_SHAPE($,$,#283);
#11867=PRODUCT_DEFINITION_SHAPE($,$,#284);
#11868=PRODUCT_DEFINITION_SHAPE($,$,#285);
#11869=PRODUCT_DEFINITION_SHAPE($,$,#286);
#11870=PRODUCT_DEFINITION_SHAPE($,$,#287);
#11871=PRODUCT_DEFINITION_SHAPE($,$,#288);
#11872=PRODUCT_DEFINITION_SHAPE($,$,#289);
#11873=PRODUCT_DEFINITION_SHAPE($,$,#290);
#11874=PRODUCT_DEFINITION_SHAPE($,$,#291);
#11875=PRODUCT_DEFINITION_SHAPE($,$,#292);
#11876=PRODUCT_DEFINITION_SHAPE($,$,#293);
#11877=PRODUCT_DEFINITION_SHAPE($,$,#294);
#11878=PRODUCT_DEFINITION_SHAPE($,$,#295);
#11879=PRODUCT_DEFINITION_SHAPE($,$,#296);
#11880=PRODUCT_DEFINITION_SHAPE($,$,#297);
#11881=PRODUCT_DEFINITION_SHAPE($,$,#298);
#11882=PRODUCT_DEFINITION_SHAPE($,$,#299);
#11883=PRODUCT_DEFINITION_SHAPE($,$,#300);
#11884=PRODUCT_DEFINITION_SHAPE($,$,#301);
#11885=PRODUCT_DEFINITION_SHAPE($,$,#302);
#11886=PRODUCT_DEFINITION_SHAPE($,$,#303);
#11887=PRODUCT_DEFINITION_SHAPE($,$,#304);
#11888=PRODUCT_DEFINITION_SHAPE($,$,#305);
#11889=PRODUCT_DEFINITION_SHAPE($,$,#306);
#11890=PRODUCT_DEFINITION_SHAPE($,$,#307);
#11891=PRODUCT_DEFINITION_SHAPE($,$,#308);
#11892=PRODUCT_DEFINITION_SHAPE($,$,#309);
#11893=PRODUCT_DEFINITION_SHAPE($,$,#310);
#11894=PRODUCT_DEFINITION_SHAPE($,$,#311);
#11895=PRODUCT_DEFINITION_SHAPE($,$,#312);
#11896=PRODUCT_DEFINITION_SHAPE('',$,#12009);
#11897=PRODUCT_DEFINITION_SHAPE('',$,#12010);
#11898=PRODUCT_DEFINITION_SHAPE($,$,#313);
#11899=PRODUCT_DEFINITION_SHAPE('',$,#12011);
#11900=PRODUCT_DEFINITION_SHAPE('',$,#12012);
#11901=PRODUCT_DEFINITION_SHAPE('',$,#12013);
#11902=PRODUCT_DEFINITION_SHAPE('',$,#12014);
#11903=PRODUCT_DEFINITION_SHAPE('',$,#12015);
#11904=PRODUCT_DEFINITION_SHAPE('',$,#12016);
#11905=PRODUCT_DEFINITION_SHAPE('',$,#12017);
#11906=PRODUCT_DEFINITION_SHAPE($,$,#314);
#11907=PRODUCT_DEFINITION_SHAPE($,$,#315);
#11908=PRODUCT_DEFINITION_SHAPE($,$,#316);
#11909=PRODUCT_DEFINITION_SHAPE($,$,#317);
#11910=PRODUCT_DEFINITION_SHAPE($,$,#318);
#11911=PRODUCT_DEFINITION_SHAPE('',$,#12018);
#11912=PRODUCT_DEFINITION_SHAPE('',$,#12019);
#11913=PRODUCT_DEFINITION_SHAPE('',$,#12020);
#11914=PRODUCT_DEFINITION_SHAPE($,$,#319);
#11915=PRODUCT_DEFINITION_SHAPE($,$,#320);
#11916=PRODUCT_DEFINITION_SHAPE($,$,#321);
#11917=PRODUCT_DEFINITION_SHAPE($,$,#322);
#11918=PRODUCT_DEFINITION_SHAPE($,$,#323);
#11919=PRODUCT_DEFINITION_SHAPE($,$,#324);
#11920=PRODUCT_DEFINITION_SHAPE($,$,#325);
#11921=PRODUCT_DEFINITION_SHAPE($,$,#326);
#11922=PRODUCT_DEFINITION_SHAPE($,$,#327);
#11923=PRODUCT_DEFINITION_SHAPE($,$,#328);
#11924=SHAPE_REPRESENTATION('',(#6734,#7486,#7487,#7488,#7489,#7490,#7491),
#11700);
#11925=SHAPE_REPRESENTATION('',(#6735,#7253,#7254,#7255,#7256,#7257,#7258,
#7259,#7260,#7261,#7262,#7263,#7264,#7265,#7266,#7267,#7268,#7269,#7270,
#7271,#7272,#7273,#7274,#7275,#7276,#7277,#7278,#7279,#7280,#7281,#7282,
#7283,#7284,#7285,#7286,#7287,#7288,#7289,#7290,#7291,#7292,#7293,#7294,
#7295,#7296,#7297,#7298,#7299,#7300,#7301,#7302,#7303,#7304,#7305,#7306,
#7307,#7308,#7309,#7310,#7311),#11701);
#11926=SHAPE_REPRESENTATION('',(#6736),#11702);
#11927=SHAPE_REPRESENTATION('',(#6786),#11703);
#11928=SHAPE_REPRESENTATION('',(#6829),#11704);
#11929=SHAPE_REPRESENTATION('',(#6850),#11705);
#11930=SHAPE_REPRESENTATION('',(#6861),#11706);
#11931=SHAPE_REPRESENTATION('',(#6868),#11707);
#11932=SHAPE_REPRESENTATION('',(#6875),#11708);
#11933=SHAPE_REPRESENTATION('',(#6900),#11709);
#11934=SHAPE_REPRESENTATION('',(#6914),#11710);
#11935=SHAPE_REPRESENTATION('',(#6923),#11711);
#11936=SHAPE_REPRESENTATION('',(#6932),#11712);
#11937=SHAPE_REPRESENTATION('',(#6941),#11713);
#11938=SHAPE_REPRESENTATION('',(#6955),#11714);
#11939=SHAPE_REPRESENTATION('',(#6964),#11715);
#11940=SHAPE_REPRESENTATION('',(#6973),#11716);
#11941=SHAPE_REPRESENTATION('',(#6998),#11717);
#11942=SHAPE_REPRESENTATION('',(#7022),#11718);
#11943=SHAPE_REPRESENTATION('',(#7036),#11719);
#11944=SHAPE_REPRESENTATION('',(#7045),#11720);
#11945=SHAPE_REPRESENTATION('',(#7054),#11721);
#11946=SHAPE_REPRESENTATION('',(#7068),#11722);
#11947=SHAPE_REPRESENTATION('',(#7077),#11723);
#11948=SHAPE_REPRESENTATION('',(#7086),#11724);
#11949=SHAPE_REPRESENTATION('',(#7110),#11725);
#11950=SHAPE_REPRESENTATION('',(#7127),#11726);
#11951=SHAPE_REPRESENTATION('',(#7151),#11727);
#11952=SHAPE_REPRESENTATION('',(#7178),#11728);
#11953=SHAPE_REPRESENTATION('',(#7195),#11729);
#11954=SHAPE_REPRESENTATION('',(#7208),#11730);
#11955=SHAPE_REPRESENTATION('',(#7214),#11731);
#11956=SHAPE_REPRESENTATION('',(#7220),#11732);
#11957=SHAPE_REPRESENTATION('',(#7226),#11733);
#11958=SHAPE_REPRESENTATION('',(#7235),#11734);
#11959=SHAPE_REPRESENTATION('',(#7244),#11735);
#11960=SHAPE_REPRESENTATION('',(#7312,#7319),#11736);
#11961=SHAPE_REPRESENTATION('',(#7313),#11737);
#11962=SHAPE_REPRESENTATION('',(#7320,#7482,#7483,#7484,#7485),#11738);
#11963=SHAPE_REPRESENTATION('',(#7321,#7450,#7451,#7452,#7453,#7454),#11739);
#11964=SHAPE_REPRESENTATION('',(#7322),#11740);
#11965=SHAPE_REPRESENTATION('',(#7342),#11741);
#11966=SHAPE_REPRESENTATION('',(#7362),#11742);
#11967=SHAPE_REPRESENTATION('',(#7379),#11743);
#11968=SHAPE_REPRESENTATION('',(#7433),#11744);
#11969=SHAPE_REPRESENTATION('',(#7455),#11745);
#11970=SHAPE_REPRESENTATION('',(#7464),#11746);
#11971=SHAPE_REPRESENTATION('',(#7473),#11747);
#11972=PRODUCT_DEFINITION_CONTEXT('part definition',#12118,'design');
#11973=PRODUCT_DEFINITION('Shaft runout checking stand',
'PAT-094',#12021,#11972);
#11974=PRODUCT_DEFINITION('Frame and indicator','Frame and indicator',#12022,
#11972);
#11975=PRODUCT_DEFINITION('Slotted Extrusion - 20 x 20 x 400 mm',
'Slotted Extrusion - 20 x 20 x 400 mm',#12023,#11972);
#11976=PRODUCT_DEFINITION('Deck','Deck',#12024,#11972);
#11977=PRODUCT_DEFINITION('Captive slot nut','Captive slot nut',#12025,
#11972);
#11978=PRODUCT_DEFINITION('Flat Washer - M5','Flat Washer - M5',#12026,
#11972);
#11979=PRODUCT_DEFINITION('Foot strip','Foot strip',#12027,#11972);
#11980=PRODUCT_DEFINITION('Foot strip_1','Foot strip (1)',#12028,#11972);
#11981=PRODUCT_DEFINITION('Roller support','Roller support',#12029,#11972);
#11982=PRODUCT_DEFINITION('Dead axle','Dead axle',#12030,#11972);
#11983=PRODUCT_DEFINITION('Inner race spacer','Inner race spacer',#12031,
#11972);
#11984=PRODUCT_DEFINITION('Inner race spacer_1','Inner race spacer (1)',
#12032,#11972);
#11985=PRODUCT_DEFINITION('Axle keeper','Axle keeper',#12033,#11972);
#11986=PRODUCT_DEFINITION('Dead axle_1','Dead axle (1)',#12034,#11972);
#11987=PRODUCT_DEFINITION('Inner race spacer_2','Inner race spacer (3)',
#12035,#11972);
#11988=PRODUCT_DEFINITION('Axle keeper_1','Axle keeper (1)',#12036,#11972);
#11989=PRODUCT_DEFINITION('Roller support_1','Roller support (1)',#12037,
#11972);
#11990=PRODUCT_DEFINITION('M6x18 mounting screw','M6x18 mounting screw',
#12038,#11972);
#11991=PRODUCT_DEFINITION('Dead axle_2','Dead axle (2)',#12039,#11972);
#11992=PRODUCT_DEFINITION('Inner race spacer_3','Inner race spacer (5)',
#12040,#11972);
#11993=PRODUCT_DEFINITION('Axle keeper_2','Axle keeper (2)',#12041,#11972);
#11994=PRODUCT_DEFINITION('Dead axle_3','Dead axle (3)',#12042,#11972);
#11995=PRODUCT_DEFINITION('Inner race spacer_4','Inner race spacer (7)',
#12043,#11972);
#11996=PRODUCT_DEFINITION('Axle keeper_3','Axle keeper (3)',#12044,#11972);
#11997=PRODUCT_DEFINITION('M4x10 Cap Screw','M4x10 Cap Screw',#12045,#11972);
#11998=PRODUCT_DEFINITION('Indicator pedestal','Indicator pedestal',#12046,
#11972);
#11999=PRODUCT_DEFINITION('M5x14 Cap Screw','M5x14 Cap Screw',#12047,#11972);
#12000=PRODUCT_DEFINITION('Indicator cross arm','Indicator cross arm',#12048,
#11972);
#12001=PRODUCT_DEFINITION('Socket Set Screw - M5x8',
'Socket Set Screw - M5x8',#12049,#11972);
#12002=PRODUCT_DEFINITION('Indicator envelope','Indicator envelope',#12050,
#11972);
#12003=PRODUCT_DEFINITION('Indicator dial face','Indicator dial face',#12051,
#11972);
#12004=PRODUCT_DEFINITION('Dial pointer','Dial pointer',#12052,#11972);
#12005=PRODUCT_DEFINITION('Indicator probe','Indicator probe',#12053,#11972);
#12006=PRODUCT_DEFINITION('Inner race spacer_5','Inner race spacer (2)',
#12054,#11972);
#12007=PRODUCT_DEFINITION('Inner race spacer_6','Inner race spacer (6)',
#12055,#11972);
#12008=PRODUCT_DEFINITION('Inner race spacer_7','Inner race spacer (4)',
#12056,#11972);
#12009=PRODUCT_DEFINITION('Example shaft','Example shaft (1)',#12057,#11972);
#12010=PRODUCT_DEFINITION('Example shaft_1','Example shaft',#12058,#11972);
#12011=PRODUCT_DEFINITION('Support roller','Support roller',#12059,#11972);
#12012=PRODUCT_DEFINITION('Sealed Ball Bearing - 10 x 30 x 9 mm',
'Sealed Ball Bearing - 10 x 30 x 9 mm',#12060,#11972);
#12013=PRODUCT_DEFINITION('Inner ring','Inner ring',#12061,#11972);
#12014=PRODUCT_DEFINITION('Outer ring','Outer ring',#12062,#11972);
#12015=PRODUCT_DEFINITION('Balls','Balls',#12063,#11972);
#12016=PRODUCT_DEFINITION('Cage','Cage',#12064,#11972);
#12017=PRODUCT_DEFINITION('Seals 2RS','Seals 2RS',#12065,#11972);
#12018=PRODUCT_DEFINITION('Roller tread','Roller tread',#12066,#11972);
#12019=PRODUCT_DEFINITION('Bonded outer race retainer',
'Bonded outer race retainer',#12067,#11972);
#12020=PRODUCT_DEFINITION('Bonded outer race retainer_1',
'Bonded outer race retainer (1)',#12068,#11972);
#12021=PRODUCT_DEFINITION_FORMATION('',$,#12120);
#12022=PRODUCT_DEFINITION_FORMATION('',$,#12121);
#12023=PRODUCT_DEFINITION_FORMATION('',$,#12122);
#12024=PRODUCT_DEFINITION_FORMATION('',$,#12123);
#12025=PRODUCT_DEFINITION_FORMATION('',$,#12124);
#12026=PRODUCT_DEFINITION_FORMATION('',$,#12125);
#12027=PRODUCT_DEFINITION_FORMATION('',$,#12126);
#12028=PRODUCT_DEFINITION_FORMATION('',$,#12127);
#12029=PRODUCT_DEFINITION_FORMATION('',$,#12128);
#12030=PRODUCT_DEFINITION_FORMATION('',$,#12129);
#12031=PRODUCT_DEFINITION_FORMATION('',$,#12130);
#12032=PRODUCT_DEFINITION_FORMATION('',$,#12131);
#12033=PRODUCT_DEFINITION_FORMATION('',$,#12132);
#12034=PRODUCT_DEFINITION_FORMATION('',$,#12133);
#12035=PRODUCT_DEFINITION_FORMATION('',$,#12134);
#12036=PRODUCT_DEFINITION_FORMATION('',$,#12135);
#12037=PRODUCT_DEFINITION_FORMATION('',$,#12136);
#12038=PRODUCT_DEFINITION_FORMATION('',$,#12137);
#12039=PRODUCT_DEFINITION_FORMATION('',$,#12138);
#12040=PRODUCT_DEFINITION_FORMATION('',$,#12139);
#12041=PRODUCT_DEFINITION_FORMATION('',$,#12140);
#12042=PRODUCT_DEFINITION_FORMATION('',$,#12141);
#12043=PRODUCT_DEFINITION_FORMATION('',$,#12142);
#12044=PRODUCT_DEFINITION_FORMATION('',$,#12143);
#12045=PRODUCT_DEFINITION_FORMATION('',$,#12144);
#12046=PRODUCT_DEFINITION_FORMATION('',$,#12145);
#12047=PRODUCT_DEFINITION_FORMATION('',$,#12146);
#12048=PRODUCT_DEFINITION_FORMATION('',$,#12147);
#12049=PRODUCT_DEFINITION_FORMATION('',$,#12148);
#12050=PRODUCT_DEFINITION_FORMATION('',$,#12149);
#12051=PRODUCT_DEFINITION_FORMATION('',$,#12150);
#12052=PRODUCT_DEFINITION_FORMATION('',$,#12151);
#12053=PRODUCT_DEFINITION_FORMATION('',$,#12152);
#12054=PRODUCT_DEFINITION_FORMATION('',$,#12153);
#12055=PRODUCT_DEFINITION_FORMATION('',$,#12154);
#12056=PRODUCT_DEFINITION_FORMATION('',$,#12155);
#12057=PRODUCT_DEFINITION_FORMATION('',$,#12156);
#12058=PRODUCT_DEFINITION_FORMATION('',$,#12157);
#12059=PRODUCT_DEFINITION_FORMATION('',$,#12158);
#12060=PRODUCT_DEFINITION_FORMATION('',$,#12159);
#12061=PRODUCT_DEFINITION_FORMATION('',$,#12160);
#12062=PRODUCT_DEFINITION_FORMATION('',$,#12161);
#12063=PRODUCT_DEFINITION_FORMATION('',$,#12162);
#12064=PRODUCT_DEFINITION_FORMATION('',$,#12163);
#12065=PRODUCT_DEFINITION_FORMATION('',$,#12164);
#12066=PRODUCT_DEFINITION_FORMATION('',$,#12165);
#12067=PRODUCT_DEFINITION_FORMATION('',$,#12166);
#12068=PRODUCT_DEFINITION_FORMATION('',$,#12167);
#12069=PRODUCT_RELATED_PRODUCT_CATEGORY(
'PAT-094',
'PAT-094',(#12120));
#12070=PRODUCT_RELATED_PRODUCT_CATEGORY('Frame and indicator',
'Frame and indicator',(#12121));
#12071=PRODUCT_RELATED_PRODUCT_CATEGORY(
'Slotted Extrusion - 20 x 20 x 400 mm',
'Slotted Extrusion - 20 x 20 x 400 mm',(#12122));
#12072=PRODUCT_RELATED_PRODUCT_CATEGORY('Deck','Deck',(#12123));
#12073=PRODUCT_RELATED_PRODUCT_CATEGORY('Captive slot nut',
'Captive slot nut',(#12124));
#12074=PRODUCT_RELATED_PRODUCT_CATEGORY('Flat Washer - M5',
'Flat Washer - M5',(#12125));
#12075=PRODUCT_RELATED_PRODUCT_CATEGORY('Foot strip','Foot strip',(#12126));
#12076=PRODUCT_RELATED_PRODUCT_CATEGORY('Foot strip (1)',
'Foot strip (1)',(#12127));
#12077=PRODUCT_RELATED_PRODUCT_CATEGORY('Roller support',
'Roller support',(#12128));
#12078=PRODUCT_RELATED_PRODUCT_CATEGORY('Dead axle','Dead axle',(#12129));
#12079=PRODUCT_RELATED_PRODUCT_CATEGORY('Inner race spacer',
'Inner race spacer',(#12130));
#12080=PRODUCT_RELATED_PRODUCT_CATEGORY('Inner race spacer (1)',
'Inner race spacer (1)',(#12131));
#12081=PRODUCT_RELATED_PRODUCT_CATEGORY('Axle keeper','Axle keeper',(#12132));
#12082=PRODUCT_RELATED_PRODUCT_CATEGORY('Dead axle (1)','Dead axle (1)',
(#12133));
#12083=PRODUCT_RELATED_PRODUCT_CATEGORY('Inner race spacer (3)',
'Inner race spacer (3)',(#12134));
#12084=PRODUCT_RELATED_PRODUCT_CATEGORY('Axle keeper (1)',
'Axle keeper (1)',(#12135));
#12085=PRODUCT_RELATED_PRODUCT_CATEGORY('Roller support (1)',
'Roller support (1)',(#12136));
#12086=PRODUCT_RELATED_PRODUCT_CATEGORY('M6x18 mounting screw',
'M6x18 mounting screw',(#12137));
#12087=PRODUCT_RELATED_PRODUCT_CATEGORY('Dead axle (2)','Dead axle (2)',
(#12138));
#12088=PRODUCT_RELATED_PRODUCT_CATEGORY('Inner race spacer (5)',
'Inner race spacer (5)',(#12139));
#12089=PRODUCT_RELATED_PRODUCT_CATEGORY('Axle keeper (2)',
'Axle keeper (2)',(#12140));
#12090=PRODUCT_RELATED_PRODUCT_CATEGORY('Dead axle (3)','Dead axle (3)',
(#12141));
#12091=PRODUCT_RELATED_PRODUCT_CATEGORY('Inner race spacer (7)',
'Inner race spacer (7)',(#12142));
#12092=PRODUCT_RELATED_PRODUCT_CATEGORY('Axle keeper (3)',
'Axle keeper (3)',(#12143));
#12093=PRODUCT_RELATED_PRODUCT_CATEGORY('M4x10 Cap Screw',
'M4x10 Cap Screw',(#12144));
#12094=PRODUCT_RELATED_PRODUCT_CATEGORY('Indicator pedestal',
'Indicator pedestal',(#12145));
#12095=PRODUCT_RELATED_PRODUCT_CATEGORY('M5x14 Cap Screw',
'M5x14 Cap Screw',(#12146));
#12096=PRODUCT_RELATED_PRODUCT_CATEGORY('Indicator cross arm',
'Indicator cross arm',(#12147));
#12097=PRODUCT_RELATED_PRODUCT_CATEGORY('Socket Set Screw - M5x8',
'Socket Set Screw - M5x8',(#12148));
#12098=PRODUCT_RELATED_PRODUCT_CATEGORY('Indicator envelope',
'Indicator envelope',(#12149));
#12099=PRODUCT_RELATED_PRODUCT_CATEGORY('Indicator dial face',
'Indicator dial face',(#12150));
#12100=PRODUCT_RELATED_PRODUCT_CATEGORY('Dial pointer','Dial pointer',(#12151));
#12101=PRODUCT_RELATED_PRODUCT_CATEGORY('Indicator probe',
'Indicator probe',(#12152));
#12102=PRODUCT_RELATED_PRODUCT_CATEGORY('Inner race spacer (2)',
'Inner race spacer (2)',(#12153));
#12103=PRODUCT_RELATED_PRODUCT_CATEGORY('Inner race spacer (6)',
'Inner race spacer (6)',(#12154));
#12104=PRODUCT_RELATED_PRODUCT_CATEGORY('Inner race spacer (4)',
'Inner race spacer (4)',(#12155));
#12105=PRODUCT_RELATED_PRODUCT_CATEGORY('Example shaft (1)',
'Example shaft (1)',(#12156));
#12106=PRODUCT_RELATED_PRODUCT_CATEGORY('Example shaft','Example shaft',
(#12157));
#12107=PRODUCT_RELATED_PRODUCT_CATEGORY('Support roller',
'Support roller',(#12158));
#12108=PRODUCT_RELATED_PRODUCT_CATEGORY(
'Sealed Ball Bearing - 10 x 30 x 9 mm',
'Sealed Ball Bearing - 10 x 30 x 9 mm',(#12159));
#12109=PRODUCT_RELATED_PRODUCT_CATEGORY('Inner ring','Inner ring',(#12160));
#12110=PRODUCT_RELATED_PRODUCT_CATEGORY('Outer ring','Outer ring',(#12161));
#12111=PRODUCT_RELATED_PRODUCT_CATEGORY('Balls','Balls',(#12162));
#12112=PRODUCT_RELATED_PRODUCT_CATEGORY('Cage','Cage',(#12163));
#12113=PRODUCT_RELATED_PRODUCT_CATEGORY('Seals 2RS','Seals 2RS',(#12164));
#12114=PRODUCT_RELATED_PRODUCT_CATEGORY('Roller tread','Roller tread',(#12165));
#12115=PRODUCT_RELATED_PRODUCT_CATEGORY('Bonded outer race retainer',
'Bonded outer race retainer',(#12166));
#12116=PRODUCT_RELATED_PRODUCT_CATEGORY(
'Bonded outer race retainer (1)','Bonded outer race retainer (1)',(#12167));
#12117=APPLICATION_PROTOCOL_DEFINITION('international standard',
'automotive_design',2009,#12118);
#12118=APPLICATION_CONTEXT(
'Core Data for Automotive Mechanical Design Process');
#12119=PRODUCT_CONTEXT('part definition',#12118,'mechanical');
#12120=PRODUCT('Shaft runout checking stand',
'PAT-094','Shaft runout checking stand',(#12119));
#12121=PRODUCT('Frame and indicator','Frame and indicator',
'Frame and indicator',(#12119));
#12122=PRODUCT('Slotted Extrusion - 20 x 20 x 400 mm',
'Slotted Extrusion - 20 x 20 x 400 mm',
'Slotted Extrusion - 20 x 20 x 400 mm',(#12119));
#12123=PRODUCT('Deck','Deck','Deck',(#12119));
#12124=PRODUCT('Captive slot nut','Captive slot nut','Captive slot nut',
(#12119));
#12125=PRODUCT('Flat Washer - M5','Flat Washer - M5','Flat Washer - M5',
(#12119));
#12126=PRODUCT('Foot strip','Foot strip','Foot strip',(#12119));
#12127=PRODUCT('Foot strip_1','Foot strip (1)','Foot strip',(#12119));
#12128=PRODUCT('Roller support','Roller support','Roller support',(#12119));
#12129=PRODUCT('Dead axle','Dead axle','Dead axle',(#12119));
#12130=PRODUCT('Inner race spacer','Inner race spacer',
'Inner race spacer',(#12119));
#12131=PRODUCT('Inner race spacer_1','Inner race spacer (1)',
'Inner race spacer',(#12119));
#12132=PRODUCT('Axle keeper','Axle keeper','Axle keeper',(#12119));
#12133=PRODUCT('Dead axle_1','Dead axle (1)','Dead axle',(#12119));
#12134=PRODUCT('Inner race spacer_2','Inner race spacer (3)',
'Inner race spacer',(#12119));
#12135=PRODUCT('Axle keeper_1','Axle keeper (1)','Axle keeper',(#12119));
#12136=PRODUCT('Roller support_1','Roller support (1)','Roller support',
(#12119));
#12137=PRODUCT('M6x18 mounting screw','M6x18 mounting screw',
'M6x18 mounting screw',(#12119));
#12138=PRODUCT('Dead axle_2','Dead axle (2)','Dead axle',(#12119));
#12139=PRODUCT('Inner race spacer_3','Inner race spacer (5)',
'Inner race spacer',(#12119));
#12140=PRODUCT('Axle keeper_2','Axle keeper (2)','Axle keeper',(#12119));
#12141=PRODUCT('Dead axle_3','Dead axle (3)','Dead axle',(#12119));
#12142=PRODUCT('Inner race spacer_4','Inner race spacer (7)',
'Inner race spacer',(#12119));
#12143=PRODUCT('Axle keeper_3','Axle keeper (3)','Axle keeper',(#12119));
#12144=PRODUCT('M4x10 Cap Screw','M4x10 Cap Screw','M4x10 Cap Screw',(#12119));
#12145=PRODUCT('Indicator pedestal','Indicator pedestal',
'Indicator pedestal',(#12119));
#12146=PRODUCT('M5x14 Cap Screw','M5x14 Cap Screw','M5x14 Cap Screw',(#12119));
#12147=PRODUCT('Indicator cross arm','Indicator cross arm',
'Indicator cross arm',(#12119));
#12148=PRODUCT('Socket Set Screw - M5x8','Socket Set Screw - M5x8',
'Socket Set Screw - M5x8',(#12119));
#12149=PRODUCT('Indicator envelope','Indicator envelope',
'Indicator envelope',(#12119));
#12150=PRODUCT('Indicator dial face','Indicator dial face',
'Indicator dial face',(#12119));
#12151=PRODUCT('Dial pointer','Dial pointer','Dial pointer',(#12119));
#12152=PRODUCT('Indicator probe','Indicator probe','Indicator probe',(#12119));
#12153=PRODUCT('Inner race spacer_5','Inner race spacer (2)',
'Inner race spacer',(#12119));
#12154=PRODUCT('Inner race spacer_6','Inner race spacer (6)',
'Inner race spacer',(#12119));
#12155=PRODUCT('Inner race spacer_7','Inner race spacer (4)',
'Inner race spacer',(#12119));
#12156=PRODUCT('Example shaft','Example shaft (1)','Example shaft',(#12119));
#12157=PRODUCT('Example shaft_1','Example shaft','Example shaft',(#12119));
#12158=PRODUCT('Support roller','Support roller','Support roller',(#12119));
#12159=PRODUCT('Sealed Ball Bearing - 10 x 30 x 9 mm',
'Sealed Ball Bearing - 10 x 30 x 9 mm',
'Sealed Ball Bearing - 10 x 30 x 9 mm',(#12119));
#12160=PRODUCT('Inner ring','Inner ring','Inner ring',(#12119));
#12161=PRODUCT('Outer ring','Outer ring','Outer ring',(#12119));
#12162=PRODUCT('Balls','Balls','Balls',(#12119));
#12163=PRODUCT('Cage','Cage','Cage',(#12119));
#12164=PRODUCT('Seals 2RS','Seals 2RS','Seals 2RS',(#12119));
#12165=PRODUCT('Roller tread','Roller tread','Roller tread',(#12119));
#12166=PRODUCT('Bonded outer race retainer',
'Bonded outer race retainer','Bonded outer race retainer',(#12119));
#12167=PRODUCT('Bonded outer race retainer_1',
'Bonded outer race retainer (1)','Bonded outer race retainer',(#12119));
#12168=PRESENTATION_STYLE_ASSIGNMENT((#12173));
#12169=PRESENTATION_STYLE_ASSIGNMENT((#12174));
#12170=PRESENTATION_STYLE_ASSIGNMENT((#12175));
#12171=PRESENTATION_STYLE_ASSIGNMENT((#12176));
#12172=PRESENTATION_STYLE_ASSIGNMENT((#12177));
#12173=SURFACE_STYLE_USAGE(.BOTH.,#12178);
#12174=SURFACE_STYLE_USAGE(.BOTH.,#12179);
#12175=SURFACE_STYLE_USAGE(.BOTH.,#12180);
#12176=SURFACE_STYLE_USAGE(.BOTH.,#12181);
#12177=SURFACE_STYLE_USAGE(.BOTH.,#12182);
#12178=SURFACE_SIDE_STYLE('',(#12183));
#12179=SURFACE_SIDE_STYLE('',(#12184));
#12180=SURFACE_SIDE_STYLE('',(#12185));
#12181=SURFACE_SIDE_STYLE('',(#12186));
#12182=SURFACE_SIDE_STYLE('',(#12187));
#12183=SURFACE_STYLE_FILL_AREA(#12188);
#12184=SURFACE_STYLE_FILL_AREA(#12189);
#12185=SURFACE_STYLE_FILL_AREA(#12190);
#12186=SURFACE_STYLE_FILL_AREA(#12191);
#12187=SURFACE_STYLE_FILL_AREA(#12192);
#12188=FILL_AREA_STYLE('Steel - Satin',(#12193));
#12189=FILL_AREA_STYLE('CAD Library Painted - Engineering blue',(#12194));
#12190=FILL_AREA_STYLE('CAD Library Painted - Steel gray',(#12195));
#12191=FILL_AREA_STYLE('CAD Library Painted - Deep blue',(#12196));
#12192=FILL_AREA_STYLE('CAD Library Painted - Graphite',(#12197));
#12193=FILL_AREA_STYLE_COLOUR('Steel - Satin',#12198);
#12194=FILL_AREA_STYLE_COLOUR('CAD Library Painted - Engineering blue',
#12199);
#12195=FILL_AREA_STYLE_COLOUR('CAD Library Painted - Steel gray',#12200);
#12196=FILL_AREA_STYLE_COLOUR('CAD Library Painted - Deep blue',#12201);
#12197=FILL_AREA_STYLE_COLOUR('CAD Library Painted - Graphite',#12202);
#12198=COLOUR_RGB('Steel - Satin',0.627450980392157,0.627450980392157,0.627450980392157);
#12199=COLOUR_RGB('CAD Library Painted - Engineering blue',0.12156862745098,
0.356862745098039,0.6);
#12200=COLOUR_RGB('CAD Library Painted - Steel gray',0.592156862745098,
0.631372549019608,0.67843137254902);
#12201=COLOUR_RGB('CAD Library Painted - Deep blue',0.0784313725490196,
0.203921568627451,0.349019607843137);
#12202=COLOUR_RGB('CAD Library Painted - Graphite',0.168627450980392,0.192156862745098,
0.231372549019608);
ENDSEC;
END-ISO-10303-21;
